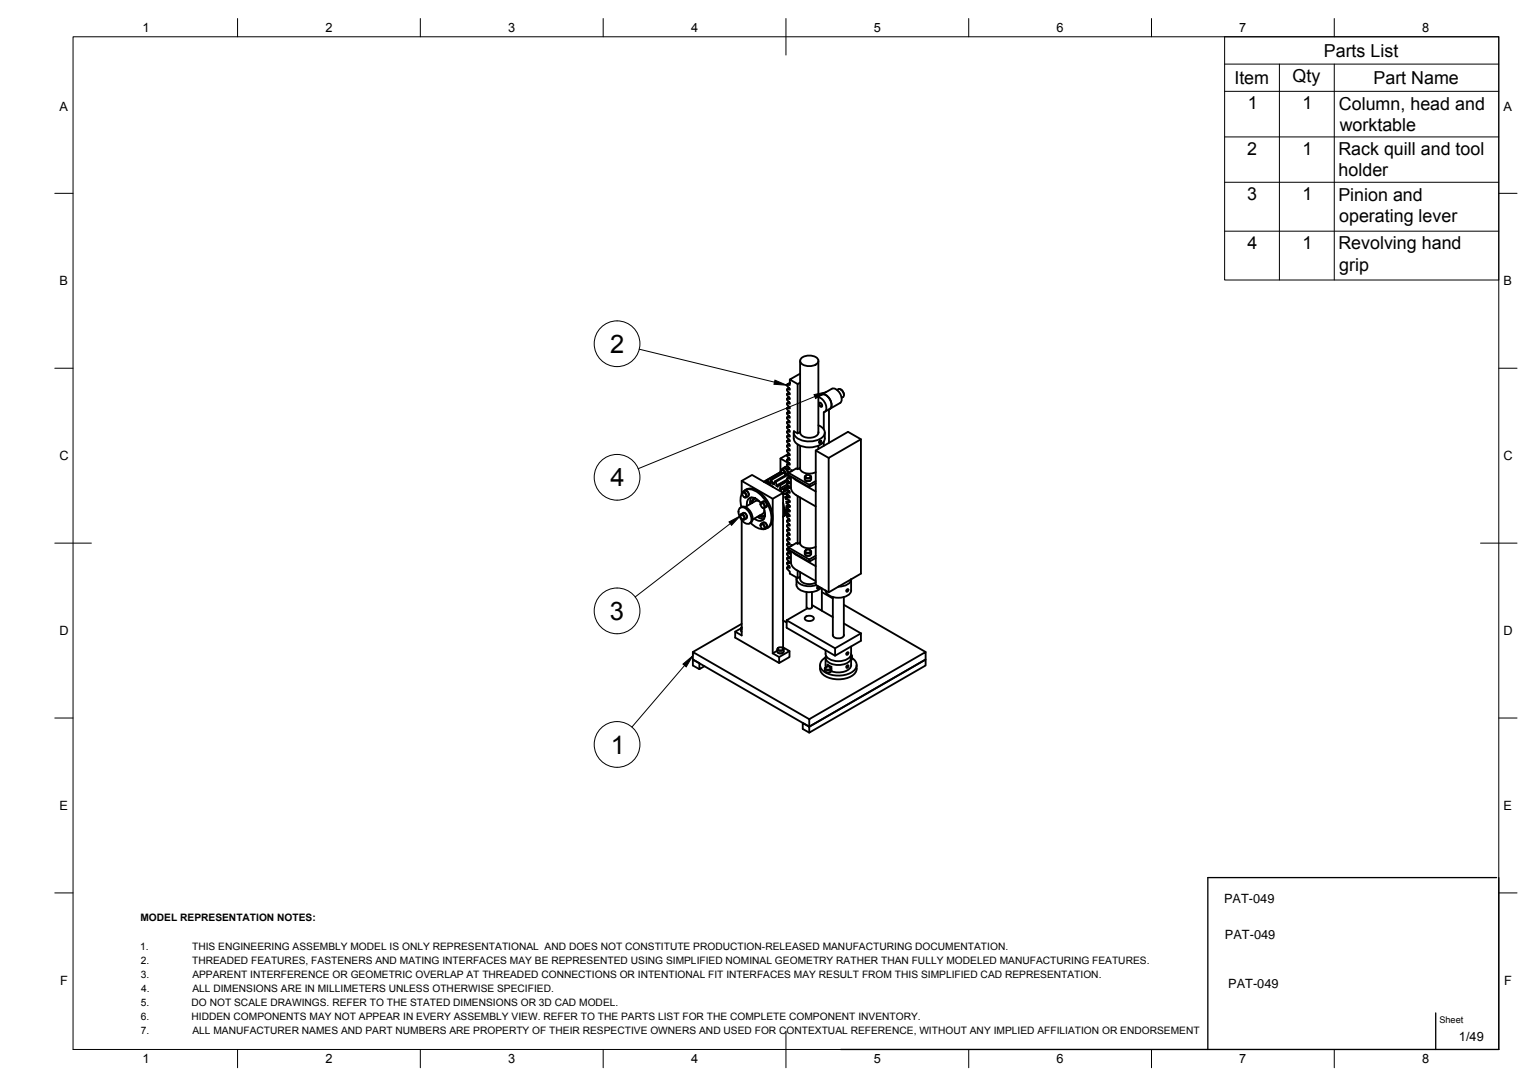
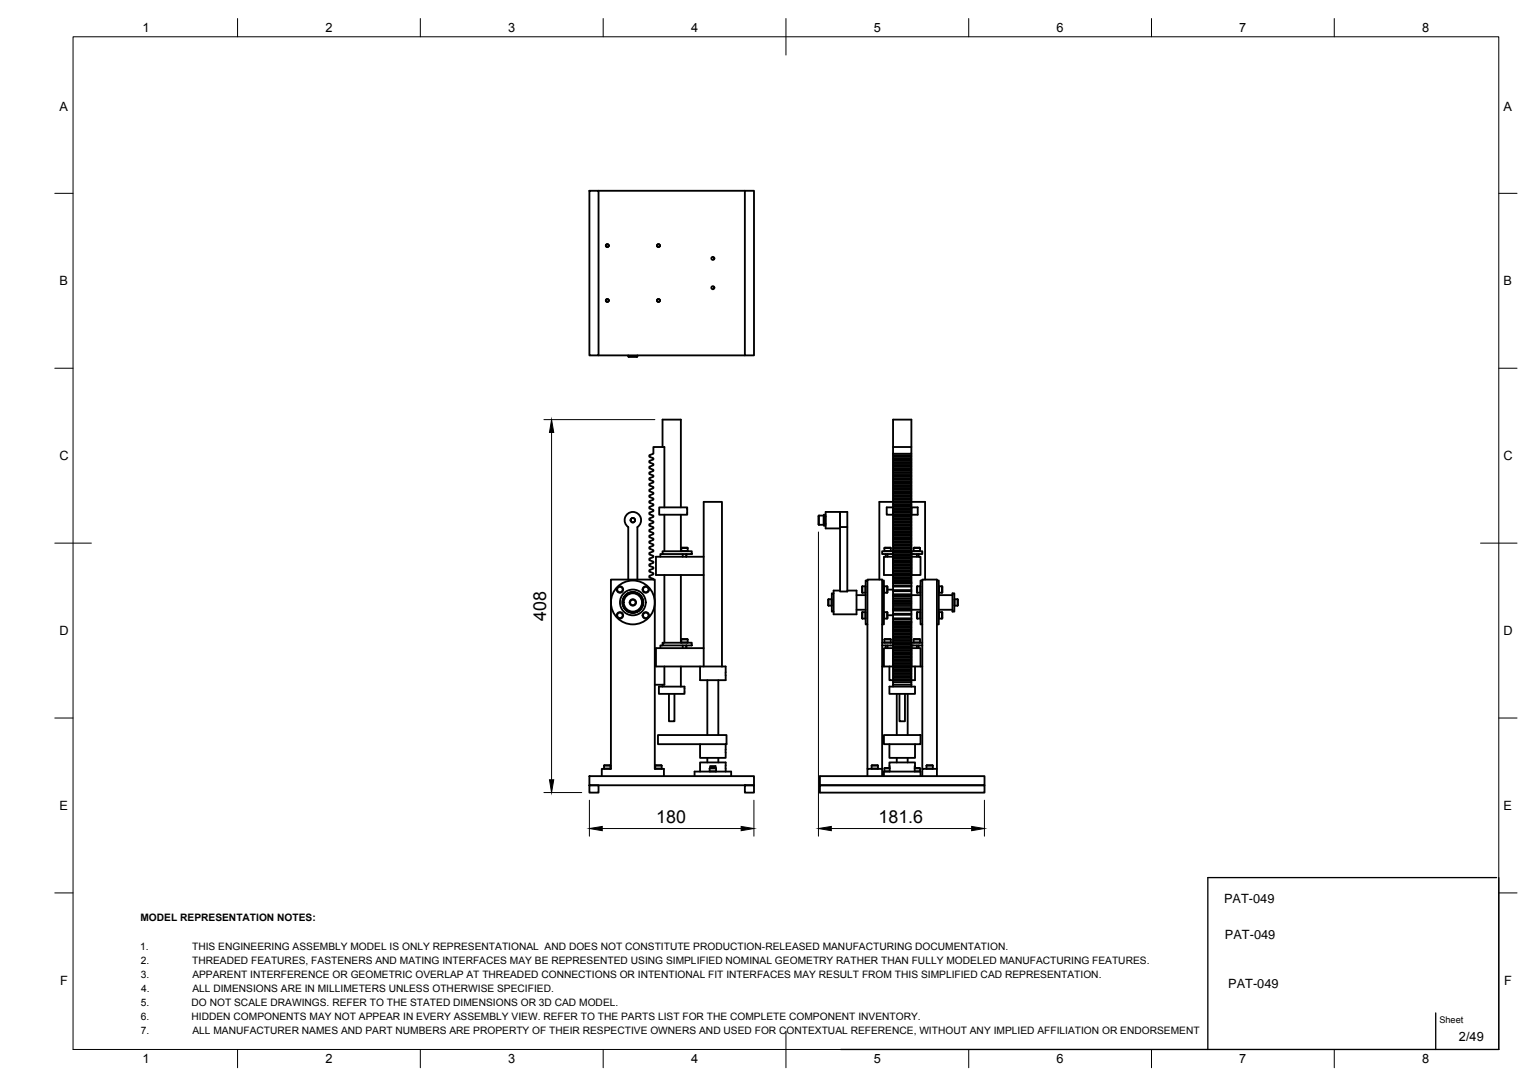
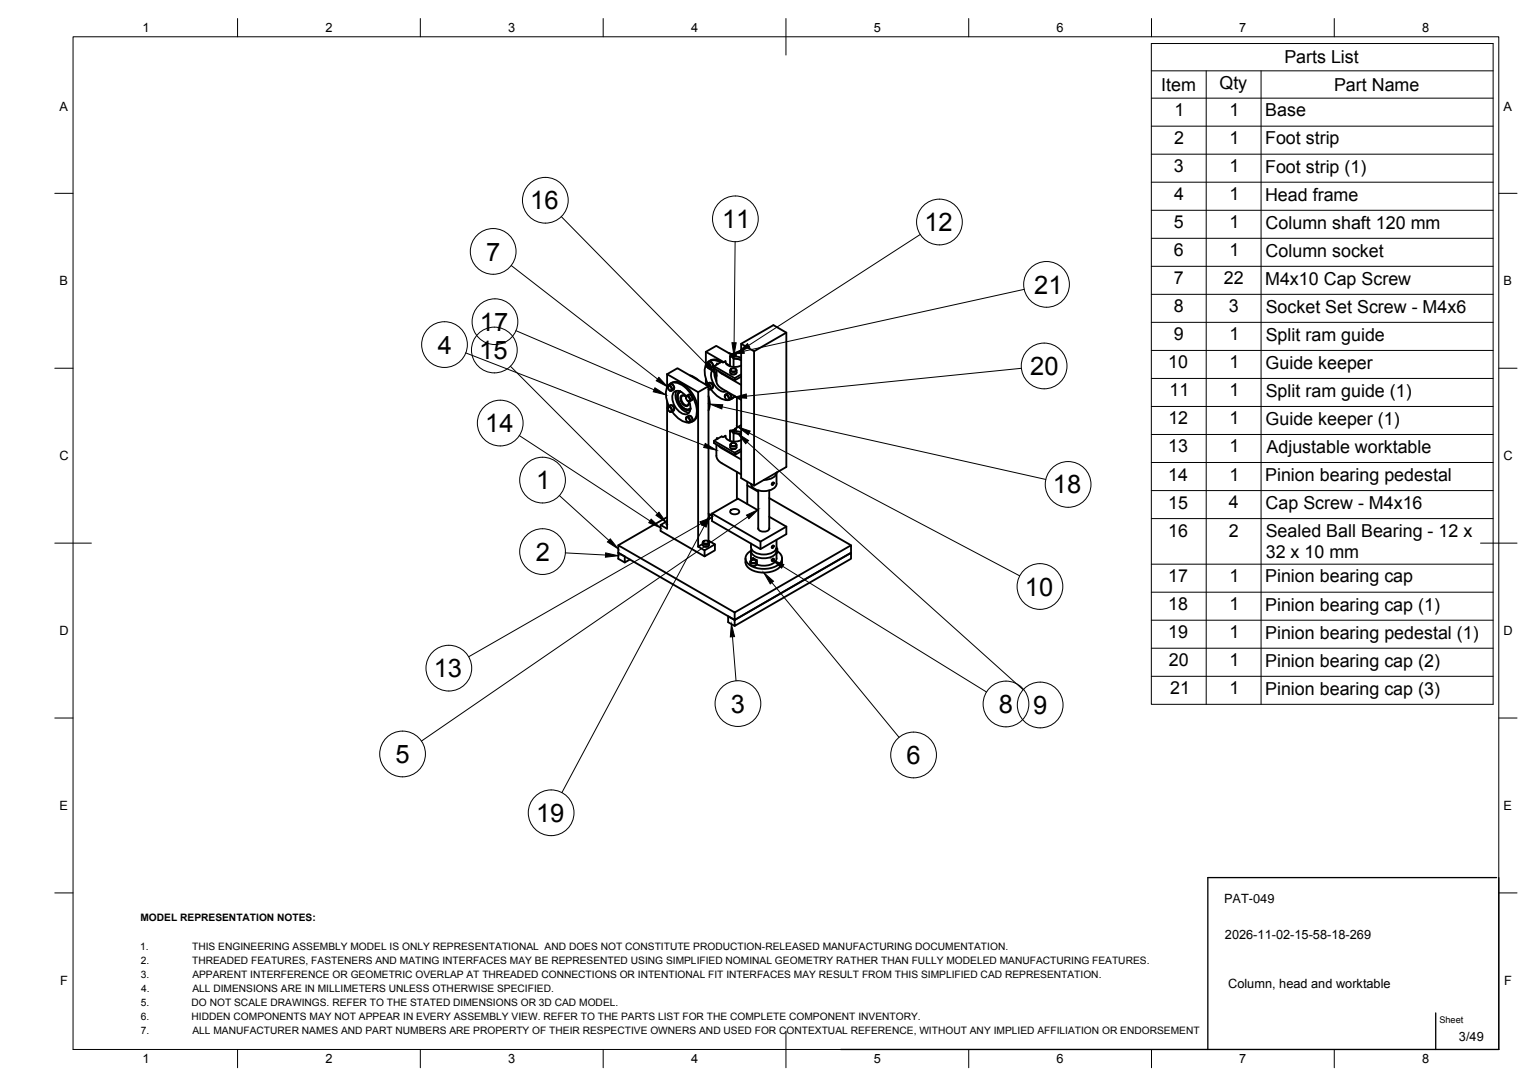
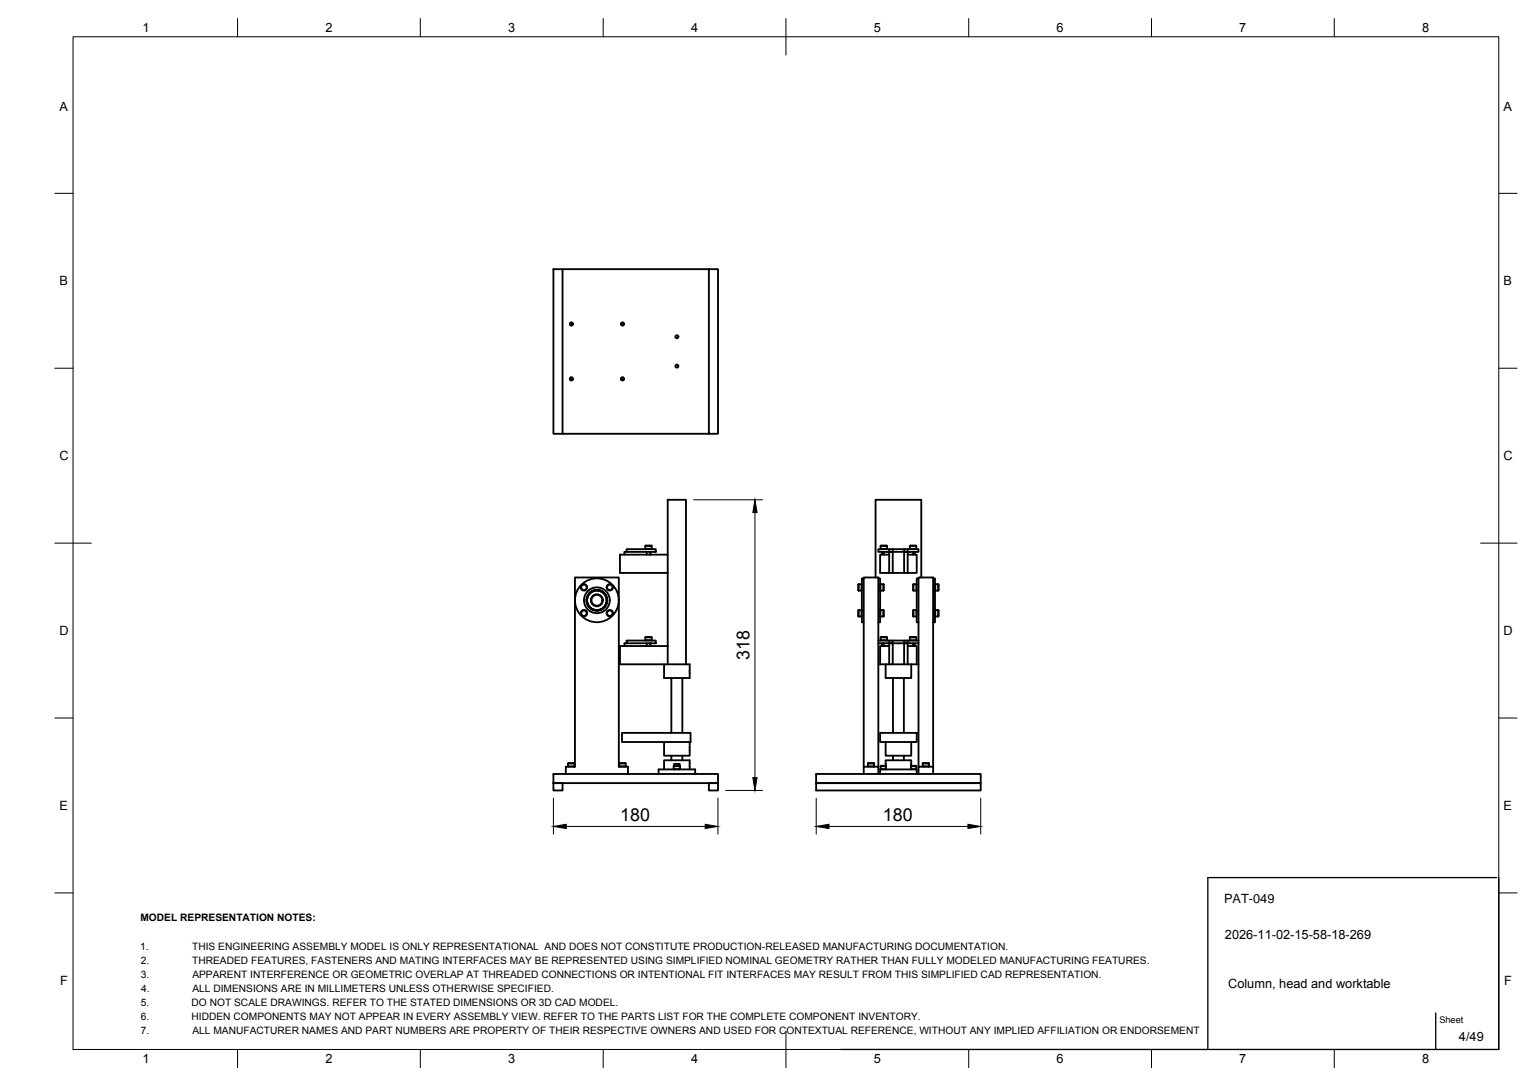
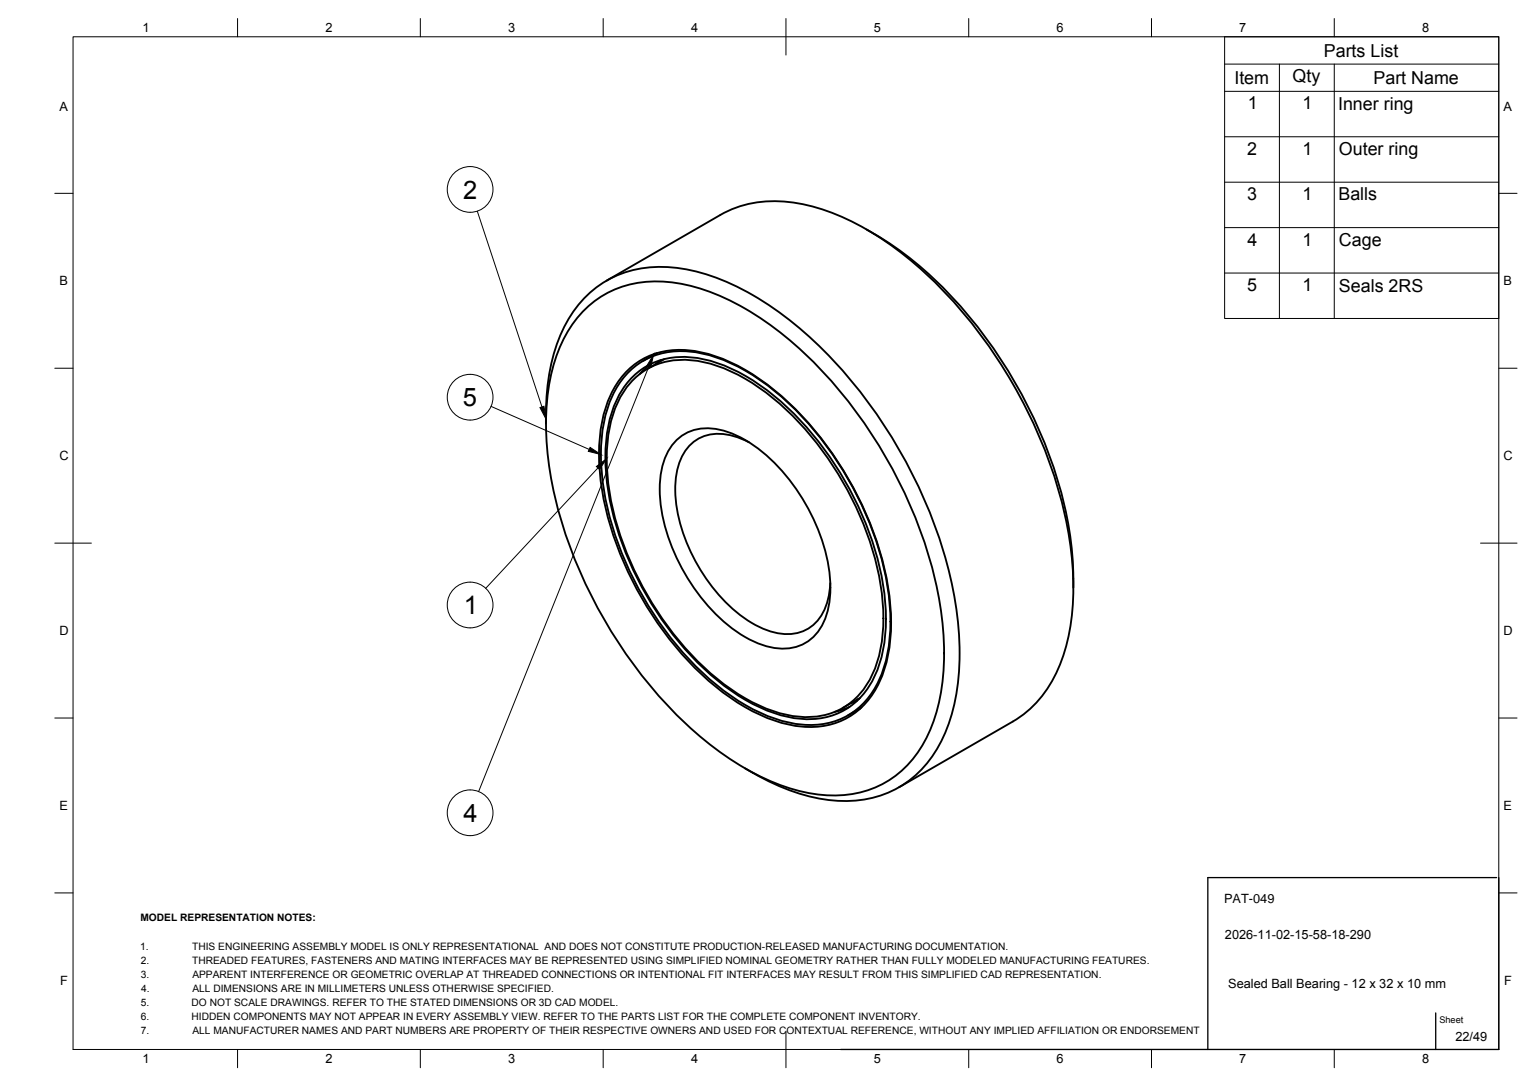
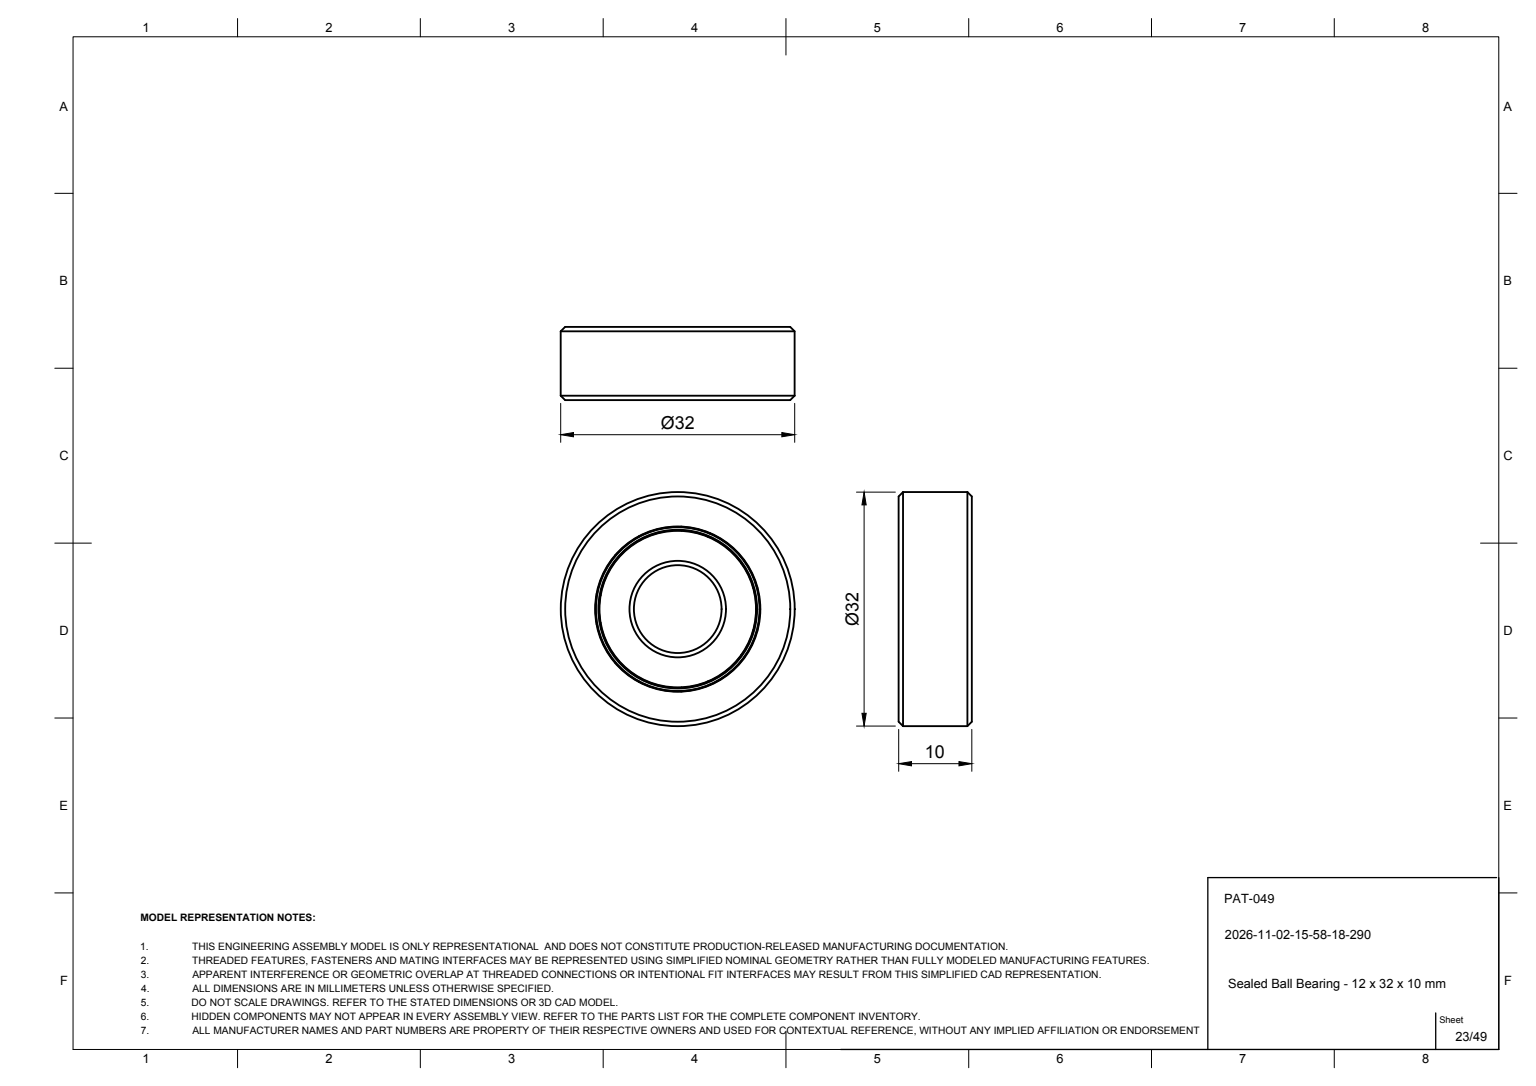
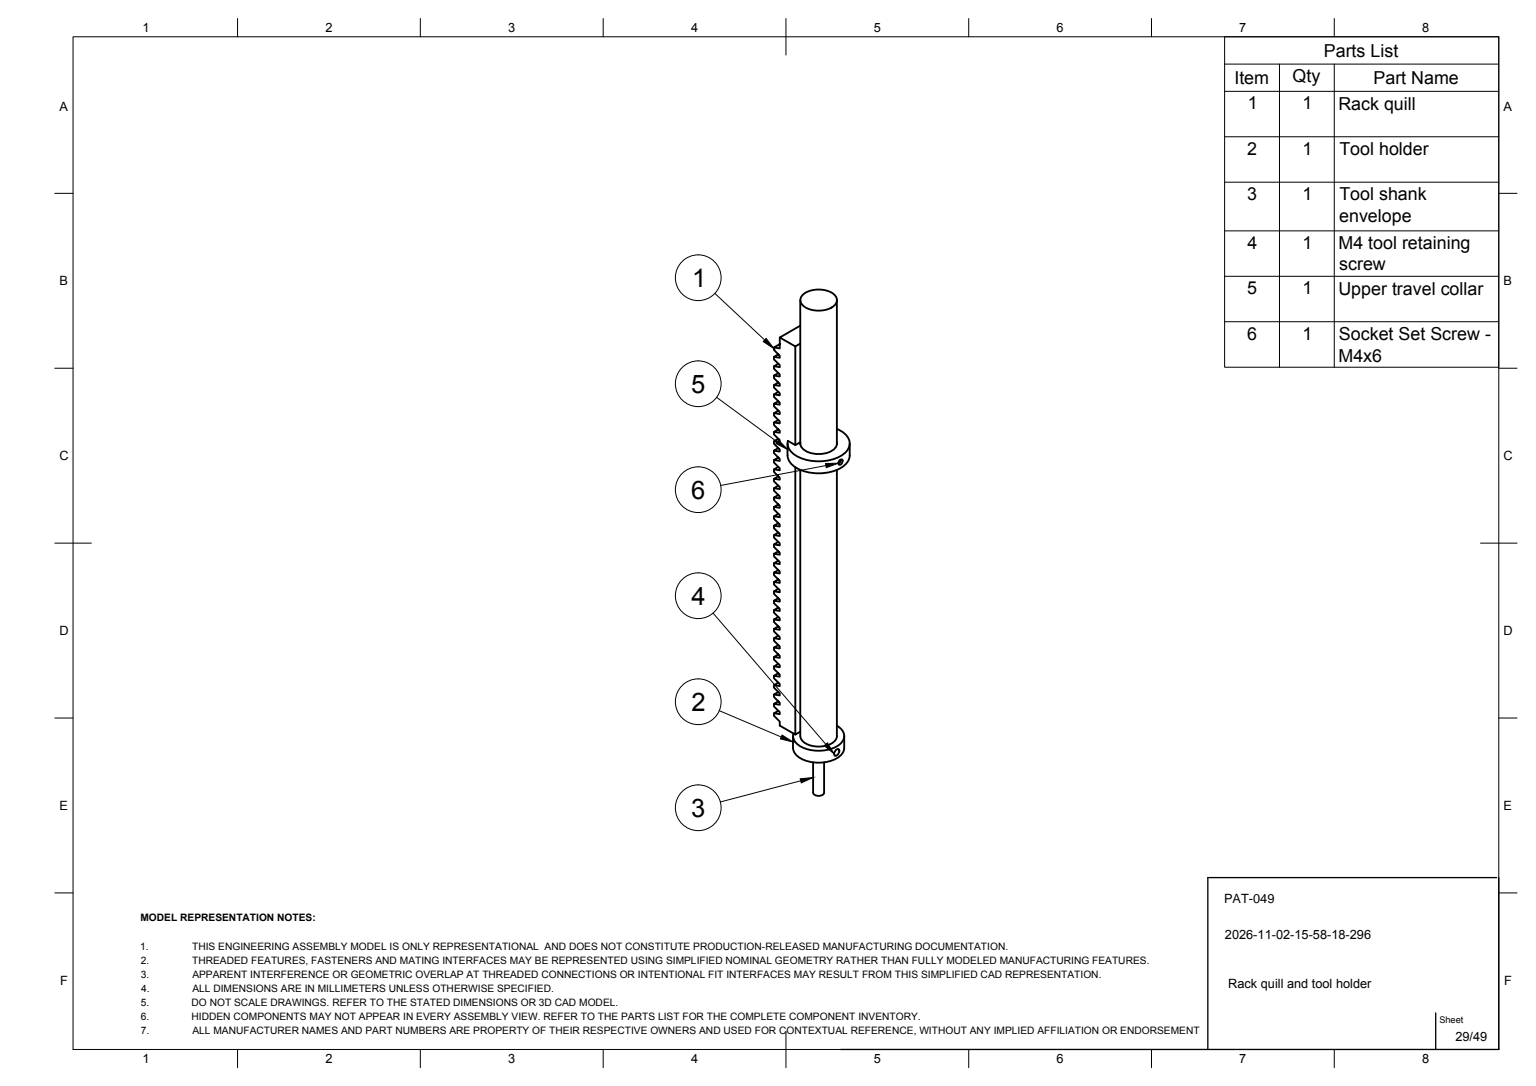
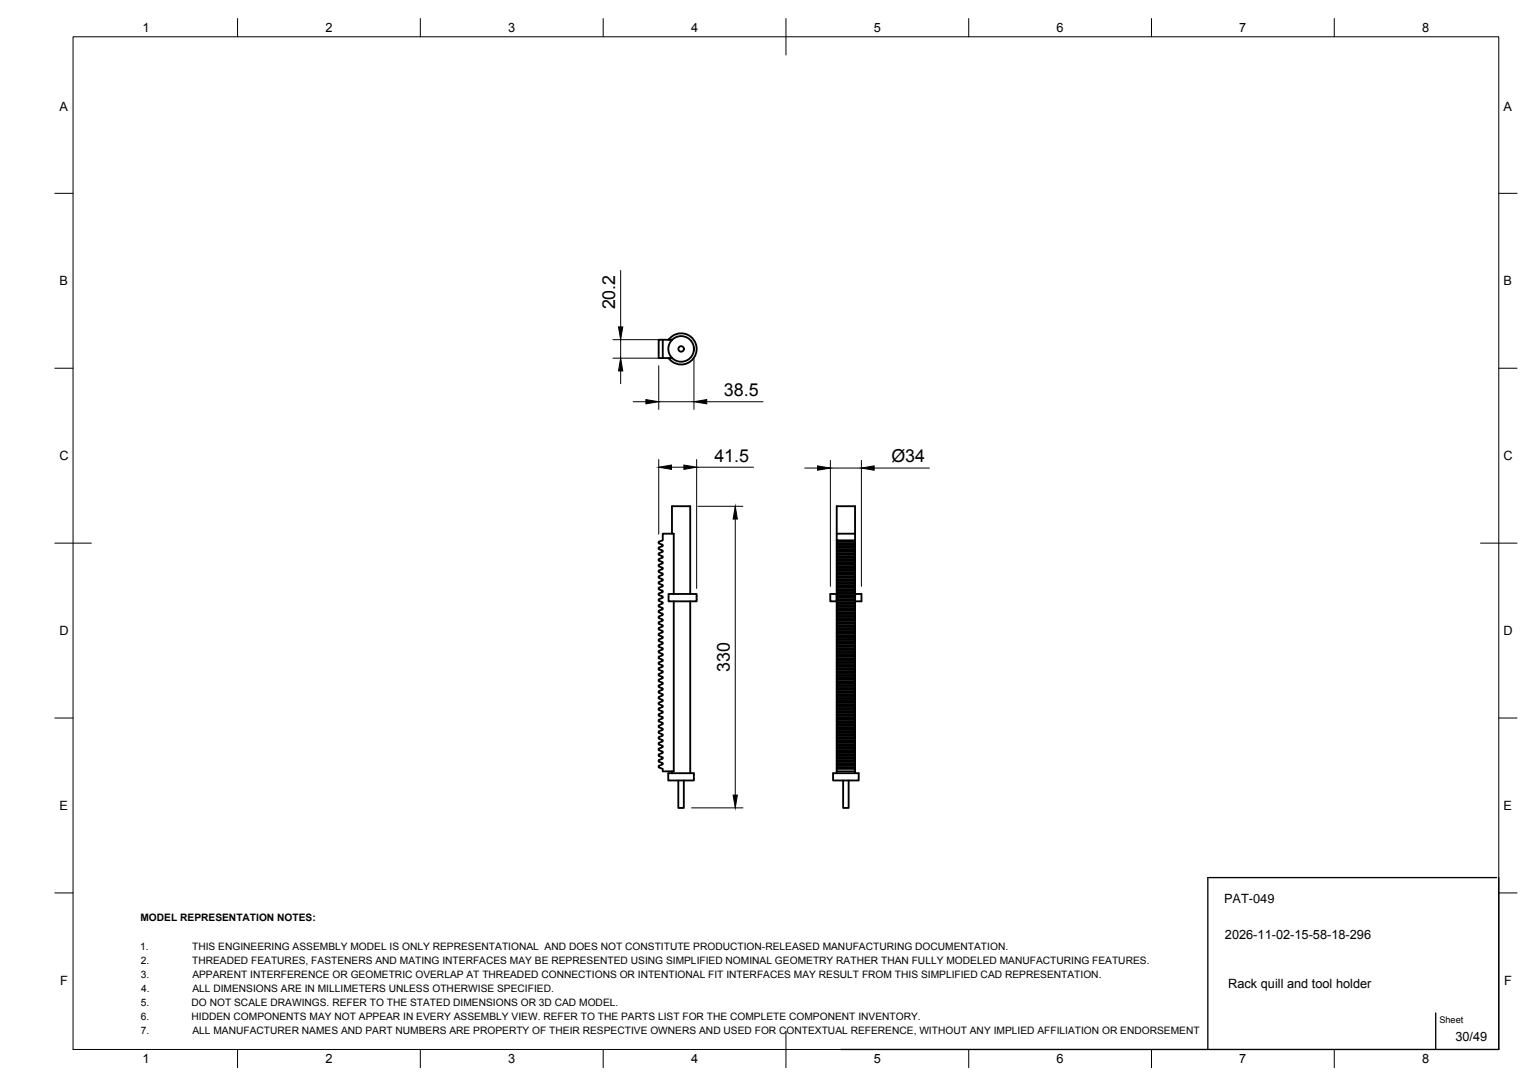
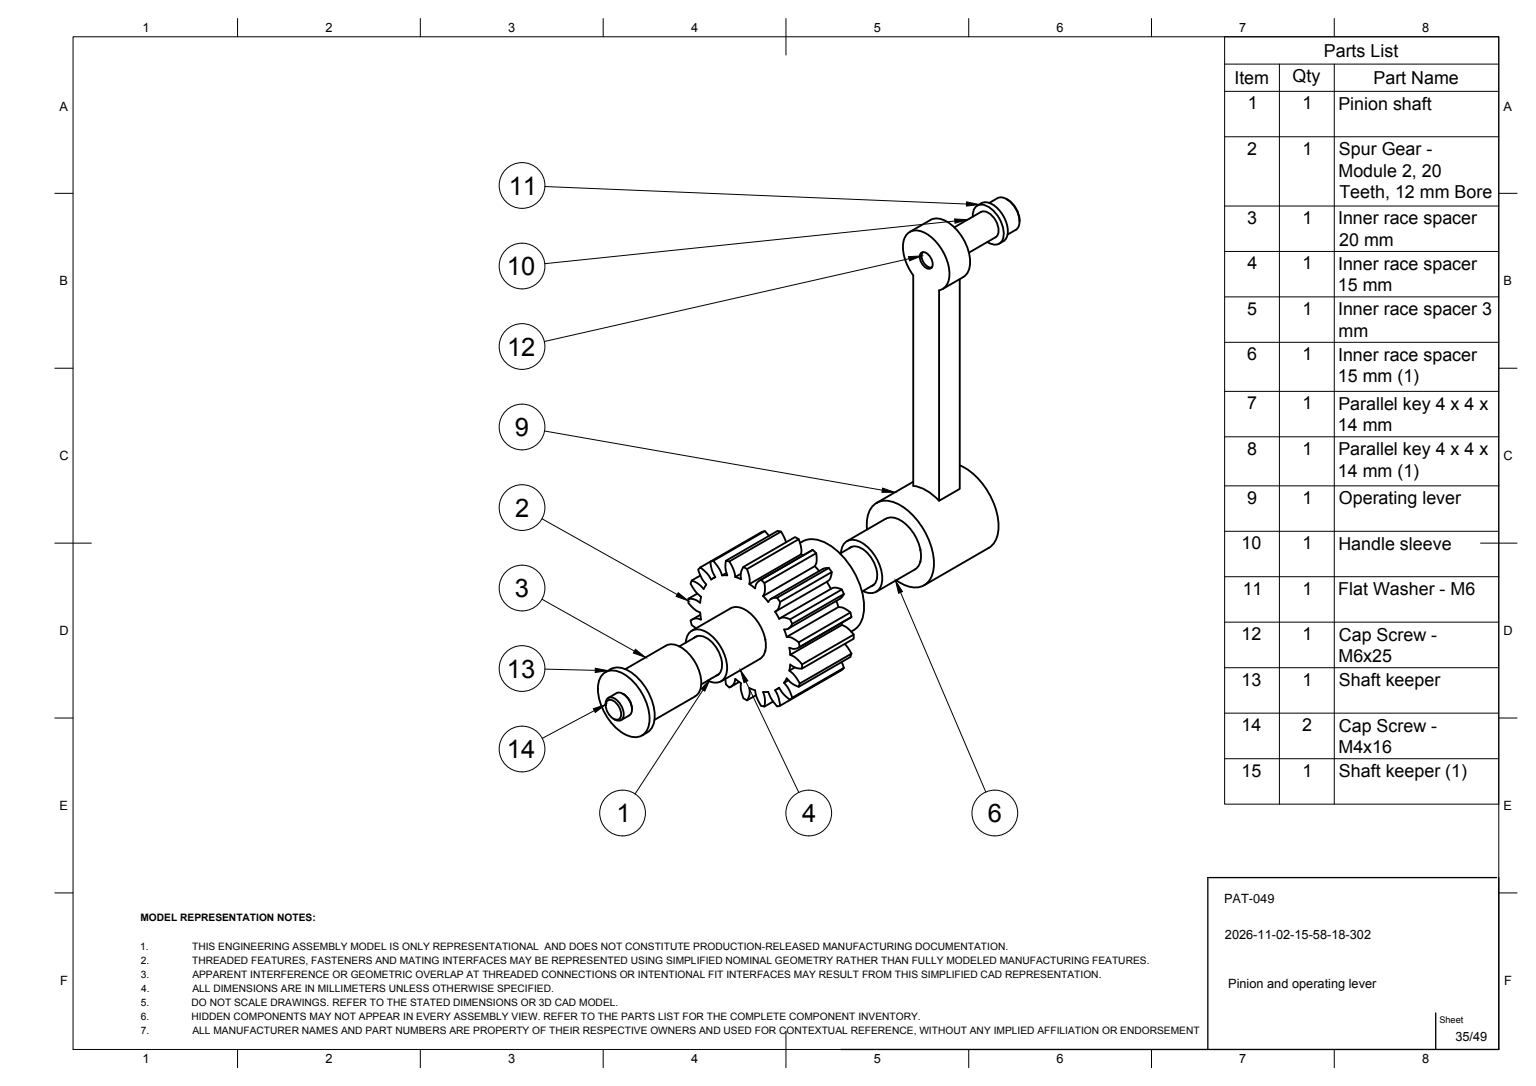
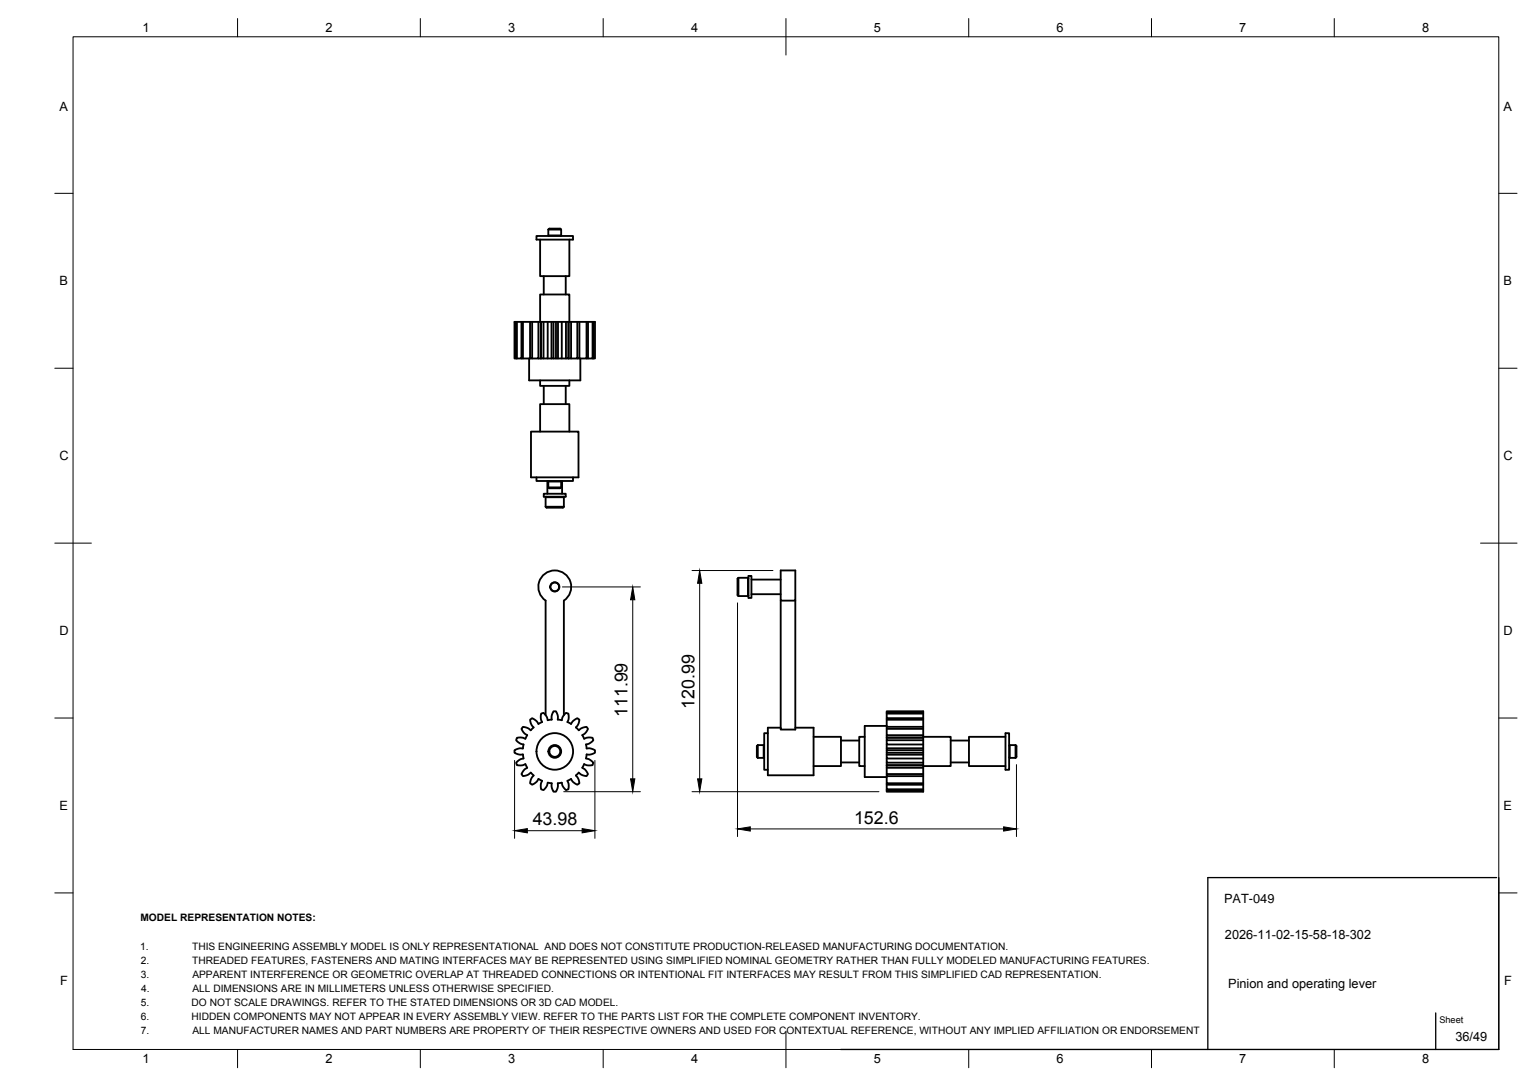
ISO-10303-21;
HEADER;
/* Generated by software containing ST-Developer
 * from STEP Tools, Inc. (www.steptools.com) 
 */

FILE_DESCRIPTION(
/* description */ ('Hand drill press frame (manual)'),
/* implementation_level */ '2;1');

FILE_NAME(
/* name */ 'PAT-049',
/* time_stamp */ '2026-10-28T03:25:28-07:00',
/* author */ (''),
/* organization */ (''),
/* preprocessor_version */ 'ST-DEVELOPER v20.2',
/* originating_system */ 'Autodesk Translation Framework v15.17.0.0',
/* authorisation */ '');

FILE_SCHEMA (('AUTOMOTIVE_DESIGN { 1 0 10303 214 3 1 1 }'));
ENDSEC;

DATA;
#10=MECHANICAL_DESIGN_GEOMETRIC_PRESENTATION_REPRESENTATION('',(#619,#620,
#621,#622,#623,#624,#625,#626,#627,#628,#629,#630,#631,#632,#633,#634,#635,
#636,#637,#638,#639,#640,#641,#642,#643,#644,#645,#646,#647,#648,#649,#650,
#651,#652,#653,#654,#655,#656,#657,#658,#659,#660,#661,#662,#663,#664,#665,
#666,#667,#668,#669,#670),#33299);
#11=(
BOUNDED_SURFACE()
B_SPLINE_SURFACE(5,1,((#24315,#24316),(#24317,#24318),(#24319,#24320),(#24321,
#24322),(#24323,#24324),(#24325,#24326),(#24327,#24328),(#24329,#24330),
(#24331,#24332),(#24333,#24334),(#24335,#24336),(#24337,#24338),(#24339,
#24340),(#24341,#24342),(#24343,#24344),(#24345,#24346),(#24347,#24348),
(#24349,#24350),(#24351,#24352),(#24353,#24354),(#24355,#24356),(#24357,
#24358),(#24359,#24360),(#24361,#24362),(#24363,#24364),(#24365,#24366),
(#24367,#24368),(#24369,#24370),(#24371,#24372),(#24373,#24374),(#24375,
#24376),(#24377,#24378),(#24379,#24380),(#24381,#24382),(#24383,#24384),
(#24385,#24386),(#24387,#24388),(#24389,#24390),(#24391,#24392),(#24393,
#24394),(#24395,#24396),(#24397,#24398),(#24399,#24400),(#24401,#24402),
(#24403,#24404),(#24405,#24406),(#24407,#24408),(#24409,#24410),(#24411,
#24412),(#24413,#24414),(#24415,#24416),(#24417,#24418),(#24419,#24420),
(#24421,#24422),(#24423,#24424),(#24425,#24426),(#24427,#24428),(#24429,
#24430),(#24431,#24432),(#24433,#24434),(#24435,#24436),(#24437,#24438),
(#24439,#24440),(#24441,#24442),(#24443,#24444),(#24445,#24446),(#24447,
#24448),(#24449,#24450),(#24451,#24452),(#24453,#24454)),.UNSPECIFIED.,
 .F.,.F.,.F.)
B_SPLINE_SURFACE_WITH_KNOTS((6,1,1,1,1,1,1,1,1,1,1,1,1,1,1,1,1,1,1,1,1,
1,1,1,1,1,1,1,1,1,1,1,1,1,1,1,1,1,1,1,1,1,1,1,1,1,1,1,1,1,1,1,1,1,1,1,1,
1,1,1,1,1,1,1,1,6),(2,2),(-1.,-0.984615384615383,-0.969230769230768,-0.953846153846152,
-0.938461538461537,-0.923076923076922,-0.907692307692306,-0.892307692307691,
-0.876923076923076,-0.86153846153846,-0.846153846153845,-0.83076923076923,
-0.815384615384614,-0.799999999999999,-0.784615384615384,-0.769230769230768,
-0.753846153846153,-0.738461538461538,-0.723076923076922,-0.707692307692307,
-0.692307692307692,-0.676923076923076,-0.661538461538461,-0.646153846153846,
-0.63076923076923,-0.615384615384615,-0.6,-0.584615384615384,-0.569230769230769,
-0.553846153846154,-0.538461538461538,-0.523076923076923,-0.507692307692308,
-0.492307692307692,-0.476923076923077,-0.461538461538462,-0.446153846153846,
-0.430769230769231,-0.415384615384615,-0.4,-0.384615384615385,-0.369230769230769,
-0.353846153846154,-0.338461538461538,-0.323076923076923,-0.307692307692308,
-0.292307692307692,-0.276923076923077,-0.261538461538462,-0.246153846153846,
-0.230769230769231,-0.215384615384615,-0.2,-0.184615384615385,-0.169230769230769,
-0.153846153846154,-0.138461538461538,-0.123076923076923,-0.107692307692308,
-0.0923076923076923,-0.0769230769230769,-0.0615384615384615,-0.0461538461538462,
-0.0307692307692308,-0.0153846153846154,0.),(-1.,1.),.UNSPECIFIED.)
GEOMETRIC_REPRESENTATION_ITEM()
RATIONAL_B_SPLINE_SURFACE(((1.,1.),(1.,1.),(1.,1.),(1.,1.),(1.,1.),(1.,
1.),(1.,1.),(1.,1.),(1.,1.),(1.,1.),(1.,1.),(1.,1.),(1.,1.),(1.,1.),(1.,
1.),(1.,1.),(1.,1.),(1.,1.),(1.,1.),(1.,1.),(1.,1.),(1.,1.),(1.,1.),(1.,
1.),(1.,1.),(1.,1.),(1.,1.),(1.,1.),(1.,1.),(1.,1.),(1.,1.),(1.,1.),(1.,
1.),(1.,1.),(1.,1.),(1.,1.),(1.,1.),(1.,1.),(1.,1.),(1.,1.),(1.,1.),(1.,
1.),(1.,1.),(1.,1.),(1.,1.),(1.,1.),(1.,1.),(1.,1.),(1.,1.),(1.,1.),(1.,
1.),(1.,1.),(1.,1.),(1.,1.),(1.,1.),(1.,1.),(1.,1.),(1.,1.),(1.,1.),(1.,
1.),(1.,1.),(1.,1.),(1.,1.),(1.,1.),(1.,1.),(1.,1.),(1.,1.),(1.,1.),(1.,
1.),(1.,1.)))
REPRESENTATION_ITEM('')
SURFACE()
);
#12=(
BOUNDED_SURFACE()
B_SPLINE_SURFACE(5,1,((#24533,#24534),(#24535,#24536),(#24537,#24538),(#24539,
#24540),(#24541,#24542),(#24543,#24544),(#24545,#24546),(#24547,#24548),
(#24549,#24550),(#24551,#24552),(#24553,#24554),(#24555,#24556),(#24557,
#24558),(#24559,#24560),(#24561,#24562),(#24563,#24564),(#24565,#24566),
(#24567,#24568),(#24569,#24570),(#24571,#24572),(#24573,#24574),(#24575,
#24576),(#24577,#24578),(#24579,#24580),(#24581,#24582),(#24583,#24584),
(#24585,#24586),(#24587,#24588),(#24589,#24590),(#24591,#24592),(#24593,
#24594),(#24595,#24596),(#24597,#24598),(#24599,#24600),(#24601,#24602),
(#24603,#24604),(#24605,#24606),(#24607,#24608),(#24609,#24610),(#24611,
#24612),(#24613,#24614),(#24615,#24616),(#24617,#24618),(#24619,#24620),
(#24621,#24622),(#24623,#24624),(#24625,#24626),(#24627,#24628),(#24629,
#24630),(#24631,#24632),(#24633,#24634),(#24635,#24636),(#24637,#24638),
(#24639,#24640),(#24641,#24642),(#24643,#24644),(#24645,#24646),(#24647,
#24648),(#24649,#24650),(#24651,#24652),(#24653,#24654),(#24655,#24656),
(#24657,#24658),(#24659,#24660),(#24661,#24662),(#24663,#24664),(#24665,
#24666),(#24667,#24668),(#24669,#24670),(#24671,#24672)),.UNSPECIFIED.,
 .F.,.F.,.F.)
B_SPLINE_SURFACE_WITH_KNOTS((6,1,1,1,1,1,1,1,1,1,1,1,1,1,1,1,1,1,1,1,1,
1,1,1,1,1,1,1,1,1,1,1,1,1,1,1,1,1,1,1,1,1,1,1,1,1,1,1,1,1,1,1,1,1,1,1,1,
1,1,1,1,1,1,1,1,6),(2,2),(-1.,-0.984615384615383,-0.969230769230768,-0.953846153846152,
-0.938461538461537,-0.923076923076922,-0.907692307692306,-0.892307692307691,
-0.876923076923076,-0.86153846153846,-0.846153846153845,-0.83076923076923,
-0.815384615384614,-0.799999999999999,-0.784615384615384,-0.769230769230768,
-0.753846153846153,-0.738461538461538,-0.723076923076922,-0.707692307692307,
-0.692307692307692,-0.676923076923076,-0.661538461538461,-0.646153846153846,
-0.63076923076923,-0.615384615384615,-0.6,-0.584615384615384,-0.569230769230769,
-0.553846153846154,-0.538461538461538,-0.523076923076923,-0.507692307692308,
-0.492307692307692,-0.476923076923077,-0.461538461538462,-0.446153846153846,
-0.430769230769231,-0.415384615384615,-0.4,-0.384615384615385,-0.369230769230769,
-0.353846153846154,-0.338461538461538,-0.323076923076923,-0.307692307692308,
-0.292307692307692,-0.276923076923077,-0.261538461538462,-0.246153846153846,
-0.230769230769231,-0.215384615384615,-0.2,-0.184615384615385,-0.169230769230769,
-0.153846153846154,-0.138461538461538,-0.123076923076923,-0.107692307692308,
-0.0923076923076923,-0.0769230769230769,-0.0615384615384615,-0.0461538461538462,
-0.0307692307692308,-0.0153846153846154,0.),(-1.,1.),.UNSPECIFIED.)
GEOMETRIC_REPRESENTATION_ITEM()
RATIONAL_B_SPLINE_SURFACE(((1.,1.),(1.,1.),(1.,1.),(1.,1.),(1.,1.),(1.,
1.),(1.,1.),(1.,1.),(1.,1.),(1.,1.),(1.,1.),(1.,1.),(1.,1.),(1.,1.),(1.,
1.),(1.,1.),(1.,1.),(1.,1.),(1.,1.),(1.,1.),(1.,1.),(1.,1.),(1.,1.),(1.,
1.),(1.,1.),(1.,1.),(1.,1.),(1.,1.),(1.,1.),(1.,1.),(1.,1.),(1.,1.),(1.,
1.),(1.,1.),(1.,1.),(1.,1.),(1.,1.),(1.,1.),(1.,1.),(1.,1.),(1.,1.),(1.,
1.),(1.,1.),(1.,1.),(1.,1.),(1.,1.),(1.,1.),(1.,1.),(1.,1.),(1.,1.),(1.,
1.),(1.,1.),(1.,1.),(1.,1.),(1.,1.),(1.,1.),(1.,1.),(1.,1.),(1.,1.),(1.,
1.),(1.,1.),(1.,1.),(1.,1.),(1.,1.),(1.,1.),(1.,1.),(1.,1.),(1.,1.),(1.,
1.),(1.,1.)))
REPRESENTATION_ITEM('')
SURFACE()
);
#13=(
BOUNDED_SURFACE()
B_SPLINE_SURFACE(5,1,((#24749,#24750),(#24751,#24752),(#24753,#24754),(#24755,
#24756),(#24757,#24758),(#24759,#24760),(#24761,#24762),(#24763,#24764),
(#24765,#24766),(#24767,#24768),(#24769,#24770),(#24771,#24772),(#24773,
#24774),(#24775,#24776),(#24777,#24778),(#24779,#24780),(#24781,#24782),
(#24783,#24784),(#24785,#24786),(#24787,#24788),(#24789,#24790),(#24791,
#24792),(#24793,#24794),(#24795,#24796),(#24797,#24798),(#24799,#24800),
(#24801,#24802),(#24803,#24804),(#24805,#24806),(#24807,#24808),(#24809,
#24810),(#24811,#24812),(#24813,#24814),(#24815,#24816),(#24817,#24818),
(#24819,#24820),(#24821,#24822),(#24823,#24824),(#24825,#24826),(#24827,
#24828),(#24829,#24830),(#24831,#24832),(#24833,#24834),(#24835,#24836),
(#24837,#24838),(#24839,#24840),(#24841,#24842),(#24843,#24844),(#24845,
#24846),(#24847,#24848),(#24849,#24850),(#24851,#24852),(#24853,#24854),
(#24855,#24856),(#24857,#24858),(#24859,#24860),(#24861,#24862),(#24863,
#24864),(#24865,#24866),(#24867,#24868),(#24869,#24870),(#24871,#24872),
(#24873,#24874),(#24875,#24876),(#24877,#24878),(#24879,#24880),(#24881,
#24882),(#24883,#24884),(#24885,#24886),(#24887,#24888)),.UNSPECIFIED.,
 .F.,.F.,.F.)
B_SPLINE_SURFACE_WITH_KNOTS((6,1,1,1,1,1,1,1,1,1,1,1,1,1,1,1,1,1,1,1,1,
1,1,1,1,1,1,1,1,1,1,1,1,1,1,1,1,1,1,1,1,1,1,1,1,1,1,1,1,1,1,1,1,1,1,1,1,
1,1,1,1,1,1,1,1,6),(2,2),(-1.,-0.984615384615383,-0.969230769230768,-0.953846153846152,
-0.938461538461537,-0.923076923076922,-0.907692307692306,-0.892307692307691,
-0.876923076923076,-0.86153846153846,-0.846153846153845,-0.83076923076923,
-0.815384615384614,-0.799999999999999,-0.784615384615384,-0.769230769230768,
-0.753846153846153,-0.738461538461538,-0.723076923076922,-0.707692307692307,
-0.692307692307692,-0.676923076923076,-0.661538461538461,-0.646153846153846,
-0.63076923076923,-0.615384615384615,-0.6,-0.584615384615384,-0.569230769230769,
-0.553846153846154,-0.538461538461538,-0.523076923076923,-0.507692307692308,
-0.492307692307692,-0.476923076923077,-0.461538461538462,-0.446153846153846,
-0.430769230769231,-0.415384615384615,-0.4,-0.384615384615385,-0.369230769230769,
-0.353846153846154,-0.338461538461538,-0.323076923076923,-0.307692307692308,
-0.292307692307692,-0.276923076923077,-0.261538461538462,-0.246153846153846,
-0.230769230769231,-0.215384615384615,-0.2,-0.184615384615385,-0.169230769230769,
-0.153846153846154,-0.138461538461538,-0.123076923076923,-0.107692307692308,
-0.0923076923076923,-0.0769230769230769,-0.0615384615384615,-0.0461538461538462,
-0.0307692307692308,-0.0153846153846154,0.),(-1.,1.),.UNSPECIFIED.)
GEOMETRIC_REPRESENTATION_ITEM()
RATIONAL_B_SPLINE_SURFACE(((1.,1.),(1.,1.),(1.,1.),(1.,1.),(1.,1.),(1.,
1.),(1.,1.),(1.,1.),(1.,1.),(1.,1.),(1.,1.),(1.,1.),(1.,1.),(1.,1.),(1.,
1.),(1.,1.),(1.,1.),(1.,1.),(1.,1.),(1.,1.),(1.,1.),(1.,1.),(1.,1.),(1.,
1.),(1.,1.),(1.,1.),(1.,1.),(1.,1.),(1.,1.),(1.,1.),(1.,1.),(1.,1.),(1.,
1.),(1.,1.),(1.,1.),(1.,1.),(1.,1.),(1.,1.),(1.,1.),(1.,1.),(1.,1.),(1.,
1.),(1.,1.),(1.,1.),(1.,1.),(1.,1.),(1.,1.),(1.,1.),(1.,1.),(1.,1.),(1.,
1.),(1.,1.),(1.,1.),(1.,1.),(1.,1.),(1.,1.),(1.,1.),(1.,1.),(1.,1.),(1.,
1.),(1.,1.),(1.,1.),(1.,1.),(1.,1.),(1.,1.),(1.,1.),(1.,1.),(1.,1.),(1.,
1.),(1.,1.)))
REPRESENTATION_ITEM('')
SURFACE()
);
#14=(
BOUNDED_SURFACE()
B_SPLINE_SURFACE(5,1,((#24965,#24966),(#24967,#24968),(#24969,#24970),(#24971,
#24972),(#24973,#24974),(#24975,#24976),(#24977,#24978),(#24979,#24980),
(#24981,#24982),(#24983,#24984),(#24985,#24986),(#24987,#24988),(#24989,
#24990),(#24991,#24992),(#24993,#24994),(#24995,#24996),(#24997,#24998),
(#24999,#25000),(#25001,#25002),(#25003,#25004),(#25005,#25006),(#25007,
#25008),(#25009,#25010),(#25011,#25012),(#25013,#25014),(#25015,#25016),
(#25017,#25018),(#25019,#25020),(#25021,#25022),(#25023,#25024),(#25025,
#25026),(#25027,#25028),(#25029,#25030),(#25031,#25032),(#25033,#25034),
(#25035,#25036),(#25037,#25038),(#25039,#25040),(#25041,#25042),(#25043,
#25044),(#25045,#25046),(#25047,#25048),(#25049,#25050),(#25051,#25052),
(#25053,#25054),(#25055,#25056),(#25057,#25058),(#25059,#25060),(#25061,
#25062),(#25063,#25064),(#25065,#25066),(#25067,#25068),(#25069,#25070),
(#25071,#25072),(#25073,#25074),(#25075,#25076),(#25077,#25078),(#25079,
#25080),(#25081,#25082),(#25083,#25084),(#25085,#25086),(#25087,#25088),
(#25089,#25090),(#25091,#25092),(#25093,#25094),(#25095,#25096),(#25097,
#25098),(#25099,#25100),(#25101,#25102),(#25103,#25104)),.UNSPECIFIED.,
 .F.,.F.,.F.)
B_SPLINE_SURFACE_WITH_KNOTS((6,1,1,1,1,1,1,1,1,1,1,1,1,1,1,1,1,1,1,1,1,
1,1,1,1,1,1,1,1,1,1,1,1,1,1,1,1,1,1,1,1,1,1,1,1,1,1,1,1,1,1,1,1,1,1,1,1,
1,1,1,1,1,1,1,1,6),(2,2),(-1.,-0.984615384615383,-0.969230769230768,-0.953846153846152,
-0.938461538461537,-0.923076923076922,-0.907692307692306,-0.892307692307691,
-0.876923076923076,-0.86153846153846,-0.846153846153845,-0.83076923076923,
-0.815384615384614,-0.799999999999999,-0.784615384615384,-0.769230769230768,
-0.753846153846153,-0.738461538461538,-0.723076923076922,-0.707692307692307,
-0.692307692307692,-0.676923076923076,-0.661538461538461,-0.646153846153846,
-0.63076923076923,-0.615384615384615,-0.6,-0.584615384615384,-0.569230769230769,
-0.553846153846154,-0.538461538461538,-0.523076923076923,-0.507692307692308,
-0.492307692307692,-0.476923076923077,-0.461538461538462,-0.446153846153846,
-0.430769230769231,-0.415384615384615,-0.4,-0.384615384615385,-0.369230769230769,
-0.353846153846154,-0.338461538461538,-0.323076923076923,-0.307692307692308,
-0.292307692307692,-0.276923076923077,-0.261538461538462,-0.246153846153846,
-0.230769230769231,-0.215384615384615,-0.2,-0.184615384615385,-0.169230769230769,
-0.153846153846154,-0.138461538461538,-0.123076923076923,-0.107692307692308,
-0.0923076923076923,-0.0769230769230769,-0.0615384615384615,-0.0461538461538462,
-0.0307692307692308,-0.0153846153846154,0.),(-1.,1.),.UNSPECIFIED.)
GEOMETRIC_REPRESENTATION_ITEM()
RATIONAL_B_SPLINE_SURFACE(((1.,1.),(1.,1.),(1.,1.),(1.,1.),(1.,1.),(1.,
1.),(1.,1.),(1.,1.),(1.,1.),(1.,1.),(1.,1.),(1.,1.),(1.,1.),(1.,1.),(1.,
1.),(1.,1.),(1.,1.),(1.,1.),(1.,1.),(1.,1.),(1.,1.),(1.,1.),(1.,1.),(1.,
1.),(1.,1.),(1.,1.),(1.,1.),(1.,1.),(1.,1.),(1.,1.),(1.,1.),(1.,1.),(1.,
1.),(1.,1.),(1.,1.),(1.,1.),(1.,1.),(1.,1.),(1.,1.),(1.,1.),(1.,1.),(1.,
1.),(1.,1.),(1.,1.),(1.,1.),(1.,1.),(1.,1.),(1.,1.),(1.,1.),(1.,1.),(1.,
1.),(1.,1.),(1.,1.),(1.,1.),(1.,1.),(1.,1.),(1.,1.),(1.,1.),(1.,1.),(1.,
1.),(1.,1.),(1.,1.),(1.,1.),(1.,1.),(1.,1.),(1.,1.),(1.,1.),(1.,1.),(1.,
1.),(1.,1.)))
REPRESENTATION_ITEM('')
SURFACE()
);
#15=(
BOUNDED_SURFACE()
B_SPLINE_SURFACE(5,1,((#25181,#25182),(#25183,#25184),(#25185,#25186),(#25187,
#25188),(#25189,#25190),(#25191,#25192),(#25193,#25194),(#25195,#25196),
(#25197,#25198),(#25199,#25200),(#25201,#25202),(#25203,#25204),(#25205,
#25206),(#25207,#25208),(#25209,#25210),(#25211,#25212),(#25213,#25214),
(#25215,#25216),(#25217,#25218),(#25219,#25220),(#25221,#25222),(#25223,
#25224),(#25225,#25226),(#25227,#25228),(#25229,#25230),(#25231,#25232),
(#25233,#25234),(#25235,#25236),(#25237,#25238),(#25239,#25240),(#25241,
#25242),(#25243,#25244),(#25245,#25246),(#25247,#25248),(#25249,#25250),
(#25251,#25252),(#25253,#25254),(#25255,#25256),(#25257,#25258),(#25259,
#25260),(#25261,#25262),(#25263,#25264),(#25265,#25266),(#25267,#25268),
(#25269,#25270),(#25271,#25272),(#25273,#25274),(#25275,#25276),(#25277,
#25278),(#25279,#25280),(#25281,#25282),(#25283,#25284),(#25285,#25286),
(#25287,#25288),(#25289,#25290),(#25291,#25292),(#25293,#25294),(#25295,
#25296),(#25297,#25298),(#25299,#25300),(#25301,#25302),(#25303,#25304),
(#25305,#25306),(#25307,#25308),(#25309,#25310),(#25311,#25312),(#25313,
#25314),(#25315,#25316),(#25317,#25318),(#25319,#25320)),.UNSPECIFIED.,
 .F.,.F.,.F.)
B_SPLINE_SURFACE_WITH_KNOTS((6,1,1,1,1,1,1,1,1,1,1,1,1,1,1,1,1,1,1,1,1,
1,1,1,1,1,1,1,1,1,1,1,1,1,1,1,1,1,1,1,1,1,1,1,1,1,1,1,1,1,1,1,1,1,1,1,1,
1,1,1,1,1,1,1,1,6),(2,2),(-1.,-0.984615384615383,-0.969230769230768,-0.953846153846152,
-0.938461538461537,-0.923076923076922,-0.907692307692306,-0.892307692307691,
-0.876923076923076,-0.86153846153846,-0.846153846153845,-0.83076923076923,
-0.815384615384614,-0.799999999999999,-0.784615384615384,-0.769230769230768,
-0.753846153846153,-0.738461538461538,-0.723076923076922,-0.707692307692307,
-0.692307692307692,-0.676923076923076,-0.661538461538461,-0.646153846153846,
-0.63076923076923,-0.615384615384615,-0.6,-0.584615384615384,-0.569230769230769,
-0.553846153846154,-0.538461538461538,-0.523076923076923,-0.507692307692308,
-0.492307692307692,-0.476923076923077,-0.461538461538462,-0.446153846153846,
-0.430769230769231,-0.415384615384615,-0.4,-0.384615384615385,-0.369230769230769,
-0.353846153846154,-0.338461538461538,-0.323076923076923,-0.307692307692308,
-0.292307692307692,-0.276923076923077,-0.261538461538462,-0.246153846153846,
-0.230769230769231,-0.215384615384615,-0.2,-0.184615384615385,-0.169230769230769,
-0.153846153846154,-0.138461538461538,-0.123076923076923,-0.107692307692308,
-0.0923076923076923,-0.0769230769230769,-0.0615384615384615,-0.0461538461538462,
-0.0307692307692308,-0.0153846153846154,0.),(-1.,1.),.UNSPECIFIED.)
GEOMETRIC_REPRESENTATION_ITEM()
RATIONAL_B_SPLINE_SURFACE(((1.,1.),(1.,1.),(1.,1.),(1.,1.),(1.,1.),(1.,
1.),(1.,1.),(1.,1.),(1.,1.),(1.,1.),(1.,1.),(1.,1.),(1.,1.),(1.,1.),(1.,
1.),(1.,1.),(1.,1.),(1.,1.),(1.,1.),(1.,1.),(1.,1.),(1.,1.),(1.,1.),(1.,
1.),(1.,1.),(1.,1.),(1.,1.),(1.,1.),(1.,1.),(1.,1.),(1.,1.),(1.,1.),(1.,
1.),(1.,1.),(1.,1.),(1.,1.),(1.,1.),(1.,1.),(1.,1.),(1.,1.),(1.,1.),(1.,
1.),(1.,1.),(1.,1.),(1.,1.),(1.,1.),(1.,1.),(1.,1.),(1.,1.),(1.,1.),(1.,
1.),(1.,1.),(1.,1.),(1.,1.),(1.,1.),(1.,1.),(1.,1.),(1.,1.),(1.,1.),(1.,
1.),(1.,1.),(1.,1.),(1.,1.),(1.,1.),(1.,1.),(1.,1.),(1.,1.),(1.,1.),(1.,
1.),(1.,1.)))
REPRESENTATION_ITEM('')
SURFACE()
);
#16=(
BOUNDED_SURFACE()
B_SPLINE_SURFACE(5,1,((#25397,#25398),(#25399,#25400),(#25401,#25402),(#25403,
#25404),(#25405,#25406),(#25407,#25408),(#25409,#25410),(#25411,#25412),
(#25413,#25414),(#25415,#25416),(#25417,#25418),(#25419,#25420),(#25421,
#25422),(#25423,#25424),(#25425,#25426),(#25427,#25428),(#25429,#25430),
(#25431,#25432),(#25433,#25434),(#25435,#25436),(#25437,#25438),(#25439,
#25440),(#25441,#25442),(#25443,#25444),(#25445,#25446),(#25447,#25448),
(#25449,#25450),(#25451,#25452),(#25453,#25454),(#25455,#25456),(#25457,
#25458),(#25459,#25460),(#25461,#25462),(#25463,#25464),(#25465,#25466),
(#25467,#25468),(#25469,#25470),(#25471,#25472),(#25473,#25474),(#25475,
#25476),(#25477,#25478),(#25479,#25480),(#25481,#25482),(#25483,#25484),
(#25485,#25486),(#25487,#25488),(#25489,#25490),(#25491,#25492),(#25493,
#25494),(#25495,#25496),(#25497,#25498),(#25499,#25500),(#25501,#25502),
(#25503,#25504),(#25505,#25506),(#25507,#25508),(#25509,#25510),(#25511,
#25512),(#25513,#25514),(#25515,#25516),(#25517,#25518),(#25519,#25520),
(#25521,#25522),(#25523,#25524),(#25525,#25526),(#25527,#25528),(#25529,
#25530),(#25531,#25532),(#25533,#25534),(#25535,#25536)),.UNSPECIFIED.,
 .F.,.F.,.F.)
B_SPLINE_SURFACE_WITH_KNOTS((6,1,1,1,1,1,1,1,1,1,1,1,1,1,1,1,1,1,1,1,1,
1,1,1,1,1,1,1,1,1,1,1,1,1,1,1,1,1,1,1,1,1,1,1,1,1,1,1,1,1,1,1,1,1,1,1,1,
1,1,1,1,1,1,1,1,6),(2,2),(-1.,-0.984615384615383,-0.969230769230768,-0.953846153846152,
-0.938461538461537,-0.923076923076922,-0.907692307692306,-0.892307692307691,
-0.876923076923076,-0.86153846153846,-0.846153846153845,-0.83076923076923,
-0.815384615384614,-0.799999999999999,-0.784615384615384,-0.769230769230768,
-0.753846153846153,-0.738461538461538,-0.723076923076922,-0.707692307692307,
-0.692307692307692,-0.676923076923076,-0.661538461538461,-0.646153846153846,
-0.63076923076923,-0.615384615384615,-0.6,-0.584615384615384,-0.569230769230769,
-0.553846153846154,-0.538461538461538,-0.523076923076923,-0.507692307692308,
-0.492307692307692,-0.476923076923077,-0.461538461538462,-0.446153846153846,
-0.430769230769231,-0.415384615384615,-0.4,-0.384615384615385,-0.369230769230769,
-0.353846153846154,-0.338461538461538,-0.323076923076923,-0.307692307692308,
-0.292307692307692,-0.276923076923077,-0.261538461538462,-0.246153846153846,
-0.230769230769231,-0.215384615384615,-0.2,-0.184615384615385,-0.169230769230769,
-0.153846153846154,-0.138461538461538,-0.123076923076923,-0.107692307692308,
-0.0923076923076923,-0.0769230769230769,-0.0615384615384615,-0.0461538461538462,
-0.0307692307692308,-0.0153846153846154,0.),(-1.,1.),.UNSPECIFIED.)
GEOMETRIC_REPRESENTATION_ITEM()
RATIONAL_B_SPLINE_SURFACE(((1.,1.),(1.,1.),(1.,1.),(1.,1.),(1.,1.),(1.,
1.),(1.,1.),(1.,1.),(1.,1.),(1.,1.),(1.,1.),(1.,1.),(1.,1.),(1.,1.),(1.,
1.),(1.,1.),(1.,1.),(1.,1.),(1.,1.),(1.,1.),(1.,1.),(1.,1.),(1.,1.),(1.,
1.),(1.,1.),(1.,1.),(1.,1.),(1.,1.),(1.,1.),(1.,1.),(1.,1.),(1.,1.),(1.,
1.),(1.,1.),(1.,1.),(1.,1.),(1.,1.),(1.,1.),(1.,1.),(1.,1.),(1.,1.),(1.,
1.),(1.,1.),(1.,1.),(1.,1.),(1.,1.),(1.,1.),(1.,1.),(1.,1.),(1.,1.),(1.,
1.),(1.,1.),(1.,1.),(1.,1.),(1.,1.),(1.,1.),(1.,1.),(1.,1.),(1.,1.),(1.,
1.),(1.,1.),(1.,1.),(1.,1.),(1.,1.),(1.,1.),(1.,1.),(1.,1.),(1.,1.),(1.,
1.),(1.,1.)))
REPRESENTATION_ITEM('')
SURFACE()
);
#17=(
BOUNDED_SURFACE()
B_SPLINE_SURFACE(5,1,((#25613,#25614),(#25615,#25616),(#25617,#25618),(#25619,
#25620),(#25621,#25622),(#25623,#25624),(#25625,#25626),(#25627,#25628),
(#25629,#25630),(#25631,#25632),(#25633,#25634),(#25635,#25636),(#25637,
#25638),(#25639,#25640),(#25641,#25642),(#25643,#25644),(#25645,#25646),
(#25647,#25648),(#25649,#25650),(#25651,#25652),(#25653,#25654),(#25655,
#25656),(#25657,#25658),(#25659,#25660),(#25661,#25662),(#25663,#25664),
(#25665,#25666),(#25667,#25668),(#25669,#25670),(#25671,#25672),(#25673,
#25674),(#25675,#25676),(#25677,#25678),(#25679,#25680),(#25681,#25682),
(#25683,#25684),(#25685,#25686),(#25687,#25688),(#25689,#25690),(#25691,
#25692),(#25693,#25694),(#25695,#25696),(#25697,#25698),(#25699,#25700),
(#25701,#25702),(#25703,#25704),(#25705,#25706),(#25707,#25708),(#25709,
#25710),(#25711,#25712),(#25713,#25714),(#25715,#25716),(#25717,#25718),
(#25719,#25720),(#25721,#25722),(#25723,#25724),(#25725,#25726),(#25727,
#25728),(#25729,#25730),(#25731,#25732),(#25733,#25734),(#25735,#25736),
(#25737,#25738),(#25739,#25740),(#25741,#25742),(#25743,#25744),(#25745,
#25746),(#25747,#25748),(#25749,#25750),(#25751,#25752)),.UNSPECIFIED.,
 .F.,.F.,.F.)
B_SPLINE_SURFACE_WITH_KNOTS((6,1,1,1,1,1,1,1,1,1,1,1,1,1,1,1,1,1,1,1,1,
1,1,1,1,1,1,1,1,1,1,1,1,1,1,1,1,1,1,1,1,1,1,1,1,1,1,1,1,1,1,1,1,1,1,1,1,
1,1,1,1,1,1,1,1,6),(2,2),(-1.,-0.984615384615383,-0.969230769230768,-0.953846153846152,
-0.938461538461537,-0.923076923076922,-0.907692307692306,-0.892307692307691,
-0.876923076923076,-0.86153846153846,-0.846153846153845,-0.83076923076923,
-0.815384615384614,-0.799999999999999,-0.784615384615384,-0.769230769230768,
-0.753846153846153,-0.738461538461538,-0.723076923076922,-0.707692307692307,
-0.692307692307692,-0.676923076923076,-0.661538461538461,-0.646153846153846,
-0.63076923076923,-0.615384615384615,-0.6,-0.584615384615384,-0.569230769230769,
-0.553846153846154,-0.538461538461538,-0.523076923076923,-0.507692307692308,
-0.492307692307692,-0.476923076923077,-0.461538461538462,-0.446153846153846,
-0.430769230769231,-0.415384615384615,-0.4,-0.384615384615385,-0.369230769230769,
-0.353846153846154,-0.338461538461538,-0.323076923076923,-0.307692307692308,
-0.292307692307692,-0.276923076923077,-0.261538461538462,-0.246153846153846,
-0.230769230769231,-0.215384615384615,-0.2,-0.184615384615385,-0.169230769230769,
-0.153846153846154,-0.138461538461538,-0.123076923076923,-0.107692307692308,
-0.0923076923076923,-0.0769230769230769,-0.0615384615384615,-0.0461538461538462,
-0.0307692307692308,-0.0153846153846154,0.),(-1.,1.),.UNSPECIFIED.)
GEOMETRIC_REPRESENTATION_ITEM()
RATIONAL_B_SPLINE_SURFACE(((1.,1.),(1.,1.),(1.,1.),(1.,1.),(1.,1.),(1.,
1.),(1.,1.),(1.,1.),(1.,1.),(1.,1.),(1.,1.),(1.,1.),(1.,1.),(1.,1.),(1.,
1.),(1.,1.),(1.,1.),(1.,1.),(1.,1.),(1.,1.),(1.,1.),(1.,1.),(1.,1.),(1.,
1.),(1.,1.),(1.,1.),(1.,1.),(1.,1.),(1.,1.),(1.,1.),(1.,1.),(1.,1.),(1.,
1.),(1.,1.),(1.,1.),(1.,1.),(1.,1.),(1.,1.),(1.,1.),(1.,1.),(1.,1.),(1.,
1.),(1.,1.),(1.,1.),(1.,1.),(1.,1.),(1.,1.),(1.,1.),(1.,1.),(1.,1.),(1.,
1.),(1.,1.),(1.,1.),(1.,1.),(1.,1.),(1.,1.),(1.,1.),(1.,1.),(1.,1.),(1.,
1.),(1.,1.),(1.,1.),(1.,1.),(1.,1.),(1.,1.),(1.,1.),(1.,1.),(1.,1.),(1.,
1.),(1.,1.)))
REPRESENTATION_ITEM('')
SURFACE()
);
#18=(
BOUNDED_SURFACE()
B_SPLINE_SURFACE(5,1,((#25829,#25830),(#25831,#25832),(#25833,#25834),(#25835,
#25836),(#25837,#25838),(#25839,#25840),(#25841,#25842),(#25843,#25844),
(#25845,#25846),(#25847,#25848),(#25849,#25850),(#25851,#25852),(#25853,
#25854),(#25855,#25856),(#25857,#25858),(#25859,#25860),(#25861,#25862),
(#25863,#25864),(#25865,#25866),(#25867,#25868),(#25869,#25870),(#25871,
#25872),(#25873,#25874),(#25875,#25876),(#25877,#25878),(#25879,#25880),
(#25881,#25882),(#25883,#25884),(#25885,#25886),(#25887,#25888),(#25889,
#25890),(#25891,#25892),(#25893,#25894),(#25895,#25896),(#25897,#25898),
(#25899,#25900),(#25901,#25902),(#25903,#25904),(#25905,#25906),(#25907,
#25908),(#25909,#25910),(#25911,#25912),(#25913,#25914),(#25915,#25916),
(#25917,#25918),(#25919,#25920),(#25921,#25922),(#25923,#25924),(#25925,
#25926),(#25927,#25928),(#25929,#25930),(#25931,#25932),(#25933,#25934),
(#25935,#25936),(#25937,#25938),(#25939,#25940),(#25941,#25942),(#25943,
#25944),(#25945,#25946),(#25947,#25948),(#25949,#25950),(#25951,#25952),
(#25953,#25954),(#25955,#25956),(#25957,#25958),(#25959,#25960),(#25961,
#25962),(#25963,#25964),(#25965,#25966),(#25967,#25968)),.UNSPECIFIED.,
 .F.,.F.,.F.)
B_SPLINE_SURFACE_WITH_KNOTS((6,1,1,1,1,1,1,1,1,1,1,1,1,1,1,1,1,1,1,1,1,
1,1,1,1,1,1,1,1,1,1,1,1,1,1,1,1,1,1,1,1,1,1,1,1,1,1,1,1,1,1,1,1,1,1,1,1,
1,1,1,1,1,1,1,1,6),(2,2),(-1.,-0.984615384615383,-0.969230769230768,-0.953846153846152,
-0.938461538461537,-0.923076923076922,-0.907692307692306,-0.892307692307691,
-0.876923076923076,-0.86153846153846,-0.846153846153845,-0.83076923076923,
-0.815384615384614,-0.799999999999999,-0.784615384615384,-0.769230769230768,
-0.753846153846153,-0.738461538461538,-0.723076923076922,-0.707692307692307,
-0.692307692307692,-0.676923076923076,-0.661538461538461,-0.646153846153846,
-0.63076923076923,-0.615384615384615,-0.6,-0.584615384615384,-0.569230769230769,
-0.553846153846154,-0.538461538461538,-0.523076923076923,-0.507692307692308,
-0.492307692307692,-0.476923076923077,-0.461538461538462,-0.446153846153846,
-0.430769230769231,-0.415384615384615,-0.4,-0.384615384615385,-0.369230769230769,
-0.353846153846154,-0.338461538461538,-0.323076923076923,-0.307692307692308,
-0.292307692307692,-0.276923076923077,-0.261538461538462,-0.246153846153846,
-0.230769230769231,-0.215384615384615,-0.2,-0.184615384615385,-0.169230769230769,
-0.153846153846154,-0.138461538461538,-0.123076923076923,-0.107692307692308,
-0.0923076923076923,-0.0769230769230769,-0.0615384615384615,-0.0461538461538462,
-0.0307692307692308,-0.0153846153846154,0.),(-1.,1.),.UNSPECIFIED.)
GEOMETRIC_REPRESENTATION_ITEM()
RATIONAL_B_SPLINE_SURFACE(((1.,1.),(1.,1.),(1.,1.),(1.,1.),(1.,1.),(1.,
1.),(1.,1.),(1.,1.),(1.,1.),(1.,1.),(1.,1.),(1.,1.),(1.,1.),(1.,1.),(1.,
1.),(1.,1.),(1.,1.),(1.,1.),(1.,1.),(1.,1.),(1.,1.),(1.,1.),(1.,1.),(1.,
1.),(1.,1.),(1.,1.),(1.,1.),(1.,1.),(1.,1.),(1.,1.),(1.,1.),(1.,1.),(1.,
1.),(1.,1.),(1.,1.),(1.,1.),(1.,1.),(1.,1.),(1.,1.),(1.,1.),(1.,1.),(1.,
1.),(1.,1.),(1.,1.),(1.,1.),(1.,1.),(1.,1.),(1.,1.),(1.,1.),(1.,1.),(1.,
1.),(1.,1.),(1.,1.),(1.,1.),(1.,1.),(1.,1.),(1.,1.),(1.,1.),(1.,1.),(1.,
1.),(1.,1.),(1.,1.),(1.,1.),(1.,1.),(1.,1.),(1.,1.),(1.,1.),(1.,1.),(1.,
1.),(1.,1.)))
REPRESENTATION_ITEM('')
SURFACE()
);
#19=(
BOUNDED_SURFACE()
B_SPLINE_SURFACE(5,1,((#26045,#26046),(#26047,#26048),(#26049,#26050),(#26051,
#26052),(#26053,#26054),(#26055,#26056),(#26057,#26058),(#26059,#26060),
(#26061,#26062),(#26063,#26064),(#26065,#26066),(#26067,#26068),(#26069,
#26070),(#26071,#26072),(#26073,#26074),(#26075,#26076),(#26077,#26078),
(#26079,#26080),(#26081,#26082),(#26083,#26084),(#26085,#26086),(#26087,
#26088),(#26089,#26090),(#26091,#26092),(#26093,#26094),(#26095,#26096),
(#26097,#26098),(#26099,#26100),(#26101,#26102),(#26103,#26104),(#26105,
#26106),(#26107,#26108),(#26109,#26110),(#26111,#26112),(#26113,#26114),
(#26115,#26116),(#26117,#26118),(#26119,#26120),(#26121,#26122),(#26123,
#26124),(#26125,#26126),(#26127,#26128),(#26129,#26130),(#26131,#26132),
(#26133,#26134),(#26135,#26136),(#26137,#26138),(#26139,#26140),(#26141,
#26142),(#26143,#26144),(#26145,#26146),(#26147,#26148),(#26149,#26150),
(#26151,#26152),(#26153,#26154),(#26155,#26156),(#26157,#26158),(#26159,
#26160),(#26161,#26162),(#26163,#26164),(#26165,#26166),(#26167,#26168),
(#26169,#26170),(#26171,#26172),(#26173,#26174),(#26175,#26176),(#26177,
#26178),(#26179,#26180),(#26181,#26182),(#26183,#26184)),.UNSPECIFIED.,
 .F.,.F.,.F.)
B_SPLINE_SURFACE_WITH_KNOTS((6,1,1,1,1,1,1,1,1,1,1,1,1,1,1,1,1,1,1,1,1,
1,1,1,1,1,1,1,1,1,1,1,1,1,1,1,1,1,1,1,1,1,1,1,1,1,1,1,1,1,1,1,1,1,1,1,1,
1,1,1,1,1,1,1,1,6),(2,2),(-1.,-0.984615384615383,-0.969230769230768,-0.953846153846152,
-0.938461538461537,-0.923076923076922,-0.907692307692306,-0.892307692307691,
-0.876923076923076,-0.86153846153846,-0.846153846153845,-0.83076923076923,
-0.815384615384614,-0.799999999999999,-0.784615384615384,-0.769230769230768,
-0.753846153846153,-0.738461538461538,-0.723076923076922,-0.707692307692307,
-0.692307692307692,-0.676923076923076,-0.661538461538461,-0.646153846153846,
-0.63076923076923,-0.615384615384615,-0.6,-0.584615384615384,-0.569230769230769,
-0.553846153846154,-0.538461538461538,-0.523076923076923,-0.507692307692308,
-0.492307692307692,-0.476923076923077,-0.461538461538462,-0.446153846153846,
-0.430769230769231,-0.415384615384615,-0.4,-0.384615384615385,-0.369230769230769,
-0.353846153846154,-0.338461538461538,-0.323076923076923,-0.307692307692308,
-0.292307692307692,-0.276923076923077,-0.261538461538462,-0.246153846153846,
-0.230769230769231,-0.215384615384615,-0.2,-0.184615384615385,-0.169230769230769,
-0.153846153846154,-0.138461538461538,-0.123076923076923,-0.107692307692308,
-0.0923076923076923,-0.0769230769230769,-0.0615384615384615,-0.0461538461538462,
-0.0307692307692308,-0.0153846153846154,0.),(-1.,1.),.UNSPECIFIED.)
GEOMETRIC_REPRESENTATION_ITEM()
RATIONAL_B_SPLINE_SURFACE(((1.,1.),(1.,1.),(1.,1.),(1.,1.),(1.,1.),(1.,
1.),(1.,1.),(1.,1.),(1.,1.),(1.,1.),(1.,1.),(1.,1.),(1.,1.),(1.,1.),(1.,
1.),(1.,1.),(1.,1.),(1.,1.),(1.,1.),(1.,1.),(1.,1.),(1.,1.),(1.,1.),(1.,
1.),(1.,1.),(1.,1.),(1.,1.),(1.,1.),(1.,1.),(1.,1.),(1.,1.),(1.,1.),(1.,
1.),(1.,1.),(1.,1.),(1.,1.),(1.,1.),(1.,1.),(1.,1.),(1.,1.),(1.,1.),(1.,
1.),(1.,1.),(1.,1.),(1.,1.),(1.,1.),(1.,1.),(1.,1.),(1.,1.),(1.,1.),(1.,
1.),(1.,1.),(1.,1.),(1.,1.),(1.,1.),(1.,1.),(1.,1.),(1.,1.),(1.,1.),(1.,
1.),(1.,1.),(1.,1.),(1.,1.),(1.,1.),(1.,1.),(1.,1.),(1.,1.),(1.,1.),(1.,
1.),(1.,1.)))
REPRESENTATION_ITEM('')
SURFACE()
);
#20=(
BOUNDED_SURFACE()
B_SPLINE_SURFACE(5,1,((#26261,#26262),(#26263,#26264),(#26265,#26266),(#26267,
#26268),(#26269,#26270),(#26271,#26272),(#26273,#26274),(#26275,#26276),
(#26277,#26278),(#26279,#26280),(#26281,#26282),(#26283,#26284),(#26285,
#26286),(#26287,#26288),(#26289,#26290),(#26291,#26292),(#26293,#26294),
(#26295,#26296),(#26297,#26298),(#26299,#26300),(#26301,#26302),(#26303,
#26304),(#26305,#26306),(#26307,#26308),(#26309,#26310),(#26311,#26312),
(#26313,#26314),(#26315,#26316),(#26317,#26318),(#26319,#26320),(#26321,
#26322),(#26323,#26324),(#26325,#26326),(#26327,#26328),(#26329,#26330),
(#26331,#26332),(#26333,#26334),(#26335,#26336),(#26337,#26338),(#26339,
#26340),(#26341,#26342),(#26343,#26344),(#26345,#26346),(#26347,#26348),
(#26349,#26350),(#26351,#26352),(#26353,#26354),(#26355,#26356),(#26357,
#26358),(#26359,#26360),(#26361,#26362),(#26363,#26364),(#26365,#26366),
(#26367,#26368),(#26369,#26370),(#26371,#26372),(#26373,#26374),(#26375,
#26376),(#26377,#26378),(#26379,#26380),(#26381,#26382),(#26383,#26384),
(#26385,#26386),(#26387,#26388),(#26389,#26390),(#26391,#26392),(#26393,
#26394),(#26395,#26396),(#26397,#26398),(#26399,#26400)),.UNSPECIFIED.,
 .F.,.F.,.F.)
B_SPLINE_SURFACE_WITH_KNOTS((6,1,1,1,1,1,1,1,1,1,1,1,1,1,1,1,1,1,1,1,1,
1,1,1,1,1,1,1,1,1,1,1,1,1,1,1,1,1,1,1,1,1,1,1,1,1,1,1,1,1,1,1,1,1,1,1,1,
1,1,1,1,1,1,1,1,6),(2,2),(-1.,-0.984615384615383,-0.969230769230768,-0.953846153846152,
-0.938461538461537,-0.923076923076922,-0.907692307692306,-0.892307692307691,
-0.876923076923076,-0.86153846153846,-0.846153846153845,-0.83076923076923,
-0.815384615384614,-0.799999999999999,-0.784615384615384,-0.769230769230768,
-0.753846153846153,-0.738461538461538,-0.723076923076922,-0.707692307692307,
-0.692307692307692,-0.676923076923076,-0.661538461538461,-0.646153846153846,
-0.63076923076923,-0.615384615384615,-0.6,-0.584615384615384,-0.569230769230769,
-0.553846153846154,-0.538461538461538,-0.523076923076923,-0.507692307692308,
-0.492307692307692,-0.476923076923077,-0.461538461538462,-0.446153846153846,
-0.430769230769231,-0.415384615384615,-0.4,-0.384615384615385,-0.369230769230769,
-0.353846153846154,-0.338461538461538,-0.323076923076923,-0.307692307692308,
-0.292307692307692,-0.276923076923077,-0.261538461538462,-0.246153846153846,
-0.230769230769231,-0.215384615384615,-0.2,-0.184615384615385,-0.169230769230769,
-0.153846153846154,-0.138461538461538,-0.123076923076923,-0.107692307692308,
-0.0923076923076923,-0.0769230769230769,-0.0615384615384615,-0.0461538461538462,
-0.0307692307692308,-0.0153846153846154,0.),(-1.,1.),.UNSPECIFIED.)
GEOMETRIC_REPRESENTATION_ITEM()
RATIONAL_B_SPLINE_SURFACE(((1.,1.),(1.,1.),(1.,1.),(1.,1.),(1.,1.),(1.,
1.),(1.,1.),(1.,1.),(1.,1.),(1.,1.),(1.,1.),(1.,1.),(1.,1.),(1.,1.),(1.,
1.),(1.,1.),(1.,1.),(1.,1.),(1.,1.),(1.,1.),(1.,1.),(1.,1.),(1.,1.),(1.,
1.),(1.,1.),(1.,1.),(1.,1.),(1.,1.),(1.,1.),(1.,1.),(1.,1.),(1.,1.),(1.,
1.),(1.,1.),(1.,1.),(1.,1.),(1.,1.),(1.,1.),(1.,1.),(1.,1.),(1.,1.),(1.,
1.),(1.,1.),(1.,1.),(1.,1.),(1.,1.),(1.,1.),(1.,1.),(1.,1.),(1.,1.),(1.,
1.),(1.,1.),(1.,1.),(1.,1.),(1.,1.),(1.,1.),(1.,1.),(1.,1.),(1.,1.),(1.,
1.),(1.,1.),(1.,1.),(1.,1.),(1.,1.),(1.,1.),(1.,1.),(1.,1.),(1.,1.),(1.,
1.),(1.,1.)))
REPRESENTATION_ITEM('')
SURFACE()
);
#21=(
BOUNDED_SURFACE()
B_SPLINE_SURFACE(5,1,((#26477,#26478),(#26479,#26480),(#26481,#26482),(#26483,
#26484),(#26485,#26486),(#26487,#26488),(#26489,#26490),(#26491,#26492),
(#26493,#26494),(#26495,#26496),(#26497,#26498),(#26499,#26500),(#26501,
#26502),(#26503,#26504),(#26505,#26506),(#26507,#26508),(#26509,#26510),
(#26511,#26512),(#26513,#26514),(#26515,#26516),(#26517,#26518),(#26519,
#26520),(#26521,#26522),(#26523,#26524),(#26525,#26526),(#26527,#26528),
(#26529,#26530),(#26531,#26532),(#26533,#26534),(#26535,#26536),(#26537,
#26538),(#26539,#26540),(#26541,#26542),(#26543,#26544),(#26545,#26546),
(#26547,#26548),(#26549,#26550),(#26551,#26552),(#26553,#26554),(#26555,
#26556),(#26557,#26558),(#26559,#26560),(#26561,#26562),(#26563,#26564),
(#26565,#26566),(#26567,#26568),(#26569,#26570),(#26571,#26572),(#26573,
#26574),(#26575,#26576),(#26577,#26578),(#26579,#26580),(#26581,#26582),
(#26583,#26584),(#26585,#26586),(#26587,#26588),(#26589,#26590),(#26591,
#26592),(#26593,#26594),(#26595,#26596),(#26597,#26598),(#26599,#26600),
(#26601,#26602),(#26603,#26604),(#26605,#26606),(#26607,#26608),(#26609,
#26610),(#26611,#26612),(#26613,#26614),(#26615,#26616)),.UNSPECIFIED.,
 .F.,.F.,.F.)
B_SPLINE_SURFACE_WITH_KNOTS((6,1,1,1,1,1,1,1,1,1,1,1,1,1,1,1,1,1,1,1,1,
1,1,1,1,1,1,1,1,1,1,1,1,1,1,1,1,1,1,1,1,1,1,1,1,1,1,1,1,1,1,1,1,1,1,1,1,
1,1,1,1,1,1,1,1,6),(2,2),(-1.,-0.984615384615383,-0.969230769230768,-0.953846153846152,
-0.938461538461537,-0.923076923076922,-0.907692307692306,-0.892307692307691,
-0.876923076923076,-0.86153846153846,-0.846153846153845,-0.83076923076923,
-0.815384615384614,-0.799999999999999,-0.784615384615384,-0.769230769230768,
-0.753846153846153,-0.738461538461538,-0.723076923076922,-0.707692307692307,
-0.692307692307692,-0.676923076923076,-0.661538461538461,-0.646153846153846,
-0.63076923076923,-0.615384615384615,-0.6,-0.584615384615384,-0.569230769230769,
-0.553846153846154,-0.538461538461538,-0.523076923076923,-0.507692307692308,
-0.492307692307692,-0.476923076923077,-0.461538461538462,-0.446153846153846,
-0.430769230769231,-0.415384615384615,-0.4,-0.384615384615385,-0.369230769230769,
-0.353846153846154,-0.338461538461538,-0.323076923076923,-0.307692307692308,
-0.292307692307692,-0.276923076923077,-0.261538461538462,-0.246153846153846,
-0.230769230769231,-0.215384615384615,-0.2,-0.184615384615385,-0.169230769230769,
-0.153846153846154,-0.138461538461538,-0.123076923076923,-0.107692307692308,
-0.0923076923076923,-0.0769230769230769,-0.0615384615384615,-0.0461538461538462,
-0.0307692307692308,-0.0153846153846154,0.),(-1.,1.),.UNSPECIFIED.)
GEOMETRIC_REPRESENTATION_ITEM()
RATIONAL_B_SPLINE_SURFACE(((1.,1.),(1.,1.),(1.,1.),(1.,1.),(1.,1.),(1.,
1.),(1.,1.),(1.,1.),(1.,1.),(1.,1.),(1.,1.),(1.,1.),(1.,1.),(1.,1.),(1.,
1.),(1.,1.),(1.,1.),(1.,1.),(1.,1.),(1.,1.),(1.,1.),(1.,1.),(1.,1.),(1.,
1.),(1.,1.),(1.,1.),(1.,1.),(1.,1.),(1.,1.),(1.,1.),(1.,1.),(1.,1.),(1.,
1.),(1.,1.),(1.,1.),(1.,1.),(1.,1.),(1.,1.),(1.,1.),(1.,1.),(1.,1.),(1.,
1.),(1.,1.),(1.,1.),(1.,1.),(1.,1.),(1.,1.),(1.,1.),(1.,1.),(1.,1.),(1.,
1.),(1.,1.),(1.,1.),(1.,1.),(1.,1.),(1.,1.),(1.,1.),(1.,1.),(1.,1.),(1.,
1.),(1.,1.),(1.,1.),(1.,1.),(1.,1.),(1.,1.),(1.,1.),(1.,1.),(1.,1.),(1.,
1.),(1.,1.)))
REPRESENTATION_ITEM('')
SURFACE()
);
#22=(
BOUNDED_SURFACE()
B_SPLINE_SURFACE(5,1,((#26693,#26694),(#26695,#26696),(#26697,#26698),(#26699,
#26700),(#26701,#26702),(#26703,#26704),(#26705,#26706),(#26707,#26708),
(#26709,#26710),(#26711,#26712),(#26713,#26714),(#26715,#26716),(#26717,
#26718),(#26719,#26720),(#26721,#26722),(#26723,#26724),(#26725,#26726),
(#26727,#26728),(#26729,#26730),(#26731,#26732),(#26733,#26734),(#26735,
#26736),(#26737,#26738),(#26739,#26740),(#26741,#26742),(#26743,#26744),
(#26745,#26746),(#26747,#26748),(#26749,#26750),(#26751,#26752),(#26753,
#26754),(#26755,#26756),(#26757,#26758),(#26759,#26760),(#26761,#26762),
(#26763,#26764),(#26765,#26766),(#26767,#26768),(#26769,#26770),(#26771,
#26772),(#26773,#26774),(#26775,#26776),(#26777,#26778),(#26779,#26780),
(#26781,#26782),(#26783,#26784),(#26785,#26786),(#26787,#26788),(#26789,
#26790),(#26791,#26792),(#26793,#26794),(#26795,#26796),(#26797,#26798),
(#26799,#26800),(#26801,#26802),(#26803,#26804),(#26805,#26806),(#26807,
#26808),(#26809,#26810),(#26811,#26812),(#26813,#26814),(#26815,#26816),
(#26817,#26818),(#26819,#26820),(#26821,#26822),(#26823,#26824),(#26825,
#26826),(#26827,#26828),(#26829,#26830),(#26831,#26832)),.UNSPECIFIED.,
 .F.,.F.,.F.)
B_SPLINE_SURFACE_WITH_KNOTS((6,1,1,1,1,1,1,1,1,1,1,1,1,1,1,1,1,1,1,1,1,
1,1,1,1,1,1,1,1,1,1,1,1,1,1,1,1,1,1,1,1,1,1,1,1,1,1,1,1,1,1,1,1,1,1,1,1,
1,1,1,1,1,1,1,1,6),(2,2),(-1.,-0.984615384615383,-0.969230769230768,-0.953846153846152,
-0.938461538461537,-0.923076923076922,-0.907692307692306,-0.892307692307691,
-0.876923076923076,-0.86153846153846,-0.846153846153845,-0.83076923076923,
-0.815384615384614,-0.799999999999999,-0.784615384615384,-0.769230769230768,
-0.753846153846153,-0.738461538461538,-0.723076923076922,-0.707692307692307,
-0.692307692307692,-0.676923076923076,-0.661538461538461,-0.646153846153846,
-0.63076923076923,-0.615384615384615,-0.6,-0.584615384615384,-0.569230769230769,
-0.553846153846154,-0.538461538461538,-0.523076923076923,-0.507692307692308,
-0.492307692307692,-0.476923076923077,-0.461538461538462,-0.446153846153846,
-0.430769230769231,-0.415384615384615,-0.4,-0.384615384615385,-0.369230769230769,
-0.353846153846154,-0.338461538461538,-0.323076923076923,-0.307692307692308,
-0.292307692307692,-0.276923076923077,-0.261538461538462,-0.246153846153846,
-0.230769230769231,-0.215384615384615,-0.2,-0.184615384615385,-0.169230769230769,
-0.153846153846154,-0.138461538461538,-0.123076923076923,-0.107692307692308,
-0.0923076923076923,-0.0769230769230769,-0.0615384615384615,-0.0461538461538462,
-0.0307692307692308,-0.0153846153846154,0.),(-1.,1.),.UNSPECIFIED.)
GEOMETRIC_REPRESENTATION_ITEM()
RATIONAL_B_SPLINE_SURFACE(((1.,1.),(1.,1.),(1.,1.),(1.,1.),(1.,1.),(1.,
1.),(1.,1.),(1.,1.),(1.,1.),(1.,1.),(1.,1.),(1.,1.),(1.,1.),(1.,1.),(1.,
1.),(1.,1.),(1.,1.),(1.,1.),(1.,1.),(1.,1.),(1.,1.),(1.,1.),(1.,1.),(1.,
1.),(1.,1.),(1.,1.),(1.,1.),(1.,1.),(1.,1.),(1.,1.),(1.,1.),(1.,1.),(1.,
1.),(1.,1.),(1.,1.),(1.,1.),(1.,1.),(1.,1.),(1.,1.),(1.,1.),(1.,1.),(1.,
1.),(1.,1.),(1.,1.),(1.,1.),(1.,1.),(1.,1.),(1.,1.),(1.,1.),(1.,1.),(1.,
1.),(1.,1.),(1.,1.),(1.,1.),(1.,1.),(1.,1.),(1.,1.),(1.,1.),(1.,1.),(1.,
1.),(1.,1.),(1.,1.),(1.,1.),(1.,1.),(1.,1.),(1.,1.),(1.,1.),(1.,1.),(1.,
1.),(1.,1.)))
REPRESENTATION_ITEM('')
SURFACE()
);
#23=(
BOUNDED_SURFACE()
B_SPLINE_SURFACE(5,1,((#26909,#26910),(#26911,#26912),(#26913,#26914),(#26915,
#26916),(#26917,#26918),(#26919,#26920),(#26921,#26922),(#26923,#26924),
(#26925,#26926),(#26927,#26928),(#26929,#26930),(#26931,#26932),(#26933,
#26934),(#26935,#26936),(#26937,#26938),(#26939,#26940),(#26941,#26942),
(#26943,#26944),(#26945,#26946),(#26947,#26948),(#26949,#26950),(#26951,
#26952),(#26953,#26954),(#26955,#26956),(#26957,#26958),(#26959,#26960),
(#26961,#26962),(#26963,#26964),(#26965,#26966),(#26967,#26968),(#26969,
#26970),(#26971,#26972),(#26973,#26974),(#26975,#26976),(#26977,#26978),
(#26979,#26980),(#26981,#26982),(#26983,#26984),(#26985,#26986),(#26987,
#26988),(#26989,#26990),(#26991,#26992),(#26993,#26994),(#26995,#26996),
(#26997,#26998),(#26999,#27000),(#27001,#27002),(#27003,#27004),(#27005,
#27006),(#27007,#27008),(#27009,#27010),(#27011,#27012),(#27013,#27014),
(#27015,#27016),(#27017,#27018),(#27019,#27020),(#27021,#27022),(#27023,
#27024),(#27025,#27026),(#27027,#27028),(#27029,#27030),(#27031,#27032),
(#27033,#27034),(#27035,#27036),(#27037,#27038),(#27039,#27040),(#27041,
#27042),(#27043,#27044),(#27045,#27046),(#27047,#27048)),.UNSPECIFIED.,
 .F.,.F.,.F.)
B_SPLINE_SURFACE_WITH_KNOTS((6,1,1,1,1,1,1,1,1,1,1,1,1,1,1,1,1,1,1,1,1,
1,1,1,1,1,1,1,1,1,1,1,1,1,1,1,1,1,1,1,1,1,1,1,1,1,1,1,1,1,1,1,1,1,1,1,1,
1,1,1,1,1,1,1,1,6),(2,2),(-1.,-0.984615384615383,-0.969230769230768,-0.953846153846152,
-0.938461538461537,-0.923076923076922,-0.907692307692306,-0.892307692307691,
-0.876923076923076,-0.86153846153846,-0.846153846153845,-0.83076923076923,
-0.815384615384614,-0.799999999999999,-0.784615384615384,-0.769230769230768,
-0.753846153846153,-0.738461538461538,-0.723076923076922,-0.707692307692307,
-0.692307692307692,-0.676923076923076,-0.661538461538461,-0.646153846153846,
-0.63076923076923,-0.615384615384615,-0.6,-0.584615384615384,-0.569230769230769,
-0.553846153846154,-0.538461538461538,-0.523076923076923,-0.507692307692308,
-0.492307692307692,-0.476923076923077,-0.461538461538462,-0.446153846153846,
-0.430769230769231,-0.415384615384615,-0.4,-0.384615384615385,-0.369230769230769,
-0.353846153846154,-0.338461538461538,-0.323076923076923,-0.307692307692308,
-0.292307692307692,-0.276923076923077,-0.261538461538462,-0.246153846153846,
-0.230769230769231,-0.215384615384615,-0.2,-0.184615384615385,-0.169230769230769,
-0.153846153846154,-0.138461538461538,-0.123076923076923,-0.107692307692308,
-0.0923076923076923,-0.0769230769230769,-0.0615384615384615,-0.0461538461538462,
-0.0307692307692308,-0.0153846153846154,0.),(-1.,1.),.UNSPECIFIED.)
GEOMETRIC_REPRESENTATION_ITEM()
RATIONAL_B_SPLINE_SURFACE(((1.,1.),(1.,1.),(1.,1.),(1.,1.),(1.,1.),(1.,
1.),(1.,1.),(1.,1.),(1.,1.),(1.,1.),(1.,1.),(1.,1.),(1.,1.),(1.,1.),(1.,
1.),(1.,1.),(1.,1.),(1.,1.),(1.,1.),(1.,1.),(1.,1.),(1.,1.),(1.,1.),(1.,
1.),(1.,1.),(1.,1.),(1.,1.),(1.,1.),(1.,1.),(1.,1.),(1.,1.),(1.,1.),(1.,
1.),(1.,1.),(1.,1.),(1.,1.),(1.,1.),(1.,1.),(1.,1.),(1.,1.),(1.,1.),(1.,
1.),(1.,1.),(1.,1.),(1.,1.),(1.,1.),(1.,1.),(1.,1.),(1.,1.),(1.,1.),(1.,
1.),(1.,1.),(1.,1.),(1.,1.),(1.,1.),(1.,1.),(1.,1.),(1.,1.),(1.,1.),(1.,
1.),(1.,1.),(1.,1.),(1.,1.),(1.,1.),(1.,1.),(1.,1.),(1.,1.),(1.,1.),(1.,
1.),(1.,1.)))
REPRESENTATION_ITEM('')
SURFACE()
);
#24=(
BOUNDED_SURFACE()
B_SPLINE_SURFACE(5,1,((#27125,#27126),(#27127,#27128),(#27129,#27130),(#27131,
#27132),(#27133,#27134),(#27135,#27136),(#27137,#27138),(#27139,#27140),
(#27141,#27142),(#27143,#27144),(#27145,#27146),(#27147,#27148),(#27149,
#27150),(#27151,#27152),(#27153,#27154),(#27155,#27156),(#27157,#27158),
(#27159,#27160),(#27161,#27162),(#27163,#27164),(#27165,#27166),(#27167,
#27168),(#27169,#27170),(#27171,#27172),(#27173,#27174),(#27175,#27176),
(#27177,#27178),(#27179,#27180),(#27181,#27182),(#27183,#27184),(#27185,
#27186),(#27187,#27188),(#27189,#27190),(#27191,#27192),(#27193,#27194),
(#27195,#27196),(#27197,#27198),(#27199,#27200),(#27201,#27202),(#27203,
#27204),(#27205,#27206),(#27207,#27208),(#27209,#27210),(#27211,#27212),
(#27213,#27214),(#27215,#27216),(#27217,#27218),(#27219,#27220),(#27221,
#27222),(#27223,#27224),(#27225,#27226),(#27227,#27228),(#27229,#27230),
(#27231,#27232),(#27233,#27234),(#27235,#27236),(#27237,#27238),(#27239,
#27240),(#27241,#27242),(#27243,#27244),(#27245,#27246),(#27247,#27248),
(#27249,#27250),(#27251,#27252),(#27253,#27254),(#27255,#27256),(#27257,
#27258),(#27259,#27260),(#27261,#27262),(#27263,#27264)),.UNSPECIFIED.,
 .F.,.F.,.F.)
B_SPLINE_SURFACE_WITH_KNOTS((6,1,1,1,1,1,1,1,1,1,1,1,1,1,1,1,1,1,1,1,1,
1,1,1,1,1,1,1,1,1,1,1,1,1,1,1,1,1,1,1,1,1,1,1,1,1,1,1,1,1,1,1,1,1,1,1,1,
1,1,1,1,1,1,1,1,6),(2,2),(-1.,-0.984615384615383,-0.969230769230768,-0.953846153846152,
-0.938461538461537,-0.923076923076922,-0.907692307692306,-0.892307692307691,
-0.876923076923076,-0.86153846153846,-0.846153846153845,-0.83076923076923,
-0.815384615384614,-0.799999999999999,-0.784615384615384,-0.769230769230768,
-0.753846153846153,-0.738461538461538,-0.723076923076922,-0.707692307692307,
-0.692307692307692,-0.676923076923076,-0.661538461538461,-0.646153846153846,
-0.63076923076923,-0.615384615384615,-0.6,-0.584615384615384,-0.569230769230769,
-0.553846153846154,-0.538461538461538,-0.523076923076923,-0.507692307692308,
-0.492307692307692,-0.476923076923077,-0.461538461538462,-0.446153846153846,
-0.430769230769231,-0.415384615384615,-0.4,-0.384615384615385,-0.369230769230769,
-0.353846153846154,-0.338461538461538,-0.323076923076923,-0.307692307692308,
-0.292307692307692,-0.276923076923077,-0.261538461538462,-0.246153846153846,
-0.230769230769231,-0.215384615384615,-0.2,-0.184615384615385,-0.169230769230769,
-0.153846153846154,-0.138461538461538,-0.123076923076923,-0.107692307692308,
-0.0923076923076923,-0.0769230769230769,-0.0615384615384615,-0.0461538461538462,
-0.0307692307692308,-0.0153846153846154,0.),(-1.,1.),.UNSPECIFIED.)
GEOMETRIC_REPRESENTATION_ITEM()
RATIONAL_B_SPLINE_SURFACE(((1.,1.),(1.,1.),(1.,1.),(1.,1.),(1.,1.),(1.,
1.),(1.,1.),(1.,1.),(1.,1.),(1.,1.),(1.,1.),(1.,1.),(1.,1.),(1.,1.),(1.,
1.),(1.,1.),(1.,1.),(1.,1.),(1.,1.),(1.,1.),(1.,1.),(1.,1.),(1.,1.),(1.,
1.),(1.,1.),(1.,1.),(1.,1.),(1.,1.),(1.,1.),(1.,1.),(1.,1.),(1.,1.),(1.,
1.),(1.,1.),(1.,1.),(1.,1.),(1.,1.),(1.,1.),(1.,1.),(1.,1.),(1.,1.),(1.,
1.),(1.,1.),(1.,1.),(1.,1.),(1.,1.),(1.,1.),(1.,1.),(1.,1.),(1.,1.),(1.,
1.),(1.,1.),(1.,1.),(1.,1.),(1.,1.),(1.,1.),(1.,1.),(1.,1.),(1.,1.),(1.,
1.),(1.,1.),(1.,1.),(1.,1.),(1.,1.),(1.,1.),(1.,1.),(1.,1.),(1.,1.),(1.,
1.),(1.,1.)))
REPRESENTATION_ITEM('')
SURFACE()
);
#25=(
BOUNDED_SURFACE()
B_SPLINE_SURFACE(5,1,((#27341,#27342),(#27343,#27344),(#27345,#27346),(#27347,
#27348),(#27349,#27350),(#27351,#27352),(#27353,#27354),(#27355,#27356),
(#27357,#27358),(#27359,#27360),(#27361,#27362),(#27363,#27364),(#27365,
#27366),(#27367,#27368),(#27369,#27370),(#27371,#27372),(#27373,#27374),
(#27375,#27376),(#27377,#27378),(#27379,#27380),(#27381,#27382),(#27383,
#27384),(#27385,#27386),(#27387,#27388),(#27389,#27390),(#27391,#27392),
(#27393,#27394),(#27395,#27396),(#27397,#27398),(#27399,#27400),(#27401,
#27402),(#27403,#27404),(#27405,#27406),(#27407,#27408),(#27409,#27410),
(#27411,#27412),(#27413,#27414),(#27415,#27416),(#27417,#27418),(#27419,
#27420),(#27421,#27422),(#27423,#27424),(#27425,#27426),(#27427,#27428),
(#27429,#27430),(#27431,#27432),(#27433,#27434),(#27435,#27436),(#27437,
#27438),(#27439,#27440),(#27441,#27442),(#27443,#27444),(#27445,#27446),
(#27447,#27448),(#27449,#27450),(#27451,#27452),(#27453,#27454),(#27455,
#27456),(#27457,#27458),(#27459,#27460),(#27461,#27462),(#27463,#27464),
(#27465,#27466),(#27467,#27468),(#27469,#27470),(#27471,#27472),(#27473,
#27474),(#27475,#27476),(#27477,#27478),(#27479,#27480)),.UNSPECIFIED.,
 .F.,.F.,.F.)
B_SPLINE_SURFACE_WITH_KNOTS((6,1,1,1,1,1,1,1,1,1,1,1,1,1,1,1,1,1,1,1,1,
1,1,1,1,1,1,1,1,1,1,1,1,1,1,1,1,1,1,1,1,1,1,1,1,1,1,1,1,1,1,1,1,1,1,1,1,
1,1,1,1,1,1,1,1,6),(2,2),(-1.,-0.984615384615383,-0.969230769230768,-0.953846153846152,
-0.938461538461537,-0.923076923076922,-0.907692307692306,-0.892307692307691,
-0.876923076923076,-0.86153846153846,-0.846153846153845,-0.83076923076923,
-0.815384615384614,-0.799999999999999,-0.784615384615384,-0.769230769230768,
-0.753846153846153,-0.738461538461538,-0.723076923076922,-0.707692307692307,
-0.692307692307692,-0.676923076923076,-0.661538461538461,-0.646153846153846,
-0.63076923076923,-0.615384615384615,-0.6,-0.584615384615384,-0.569230769230769,
-0.553846153846154,-0.538461538461538,-0.523076923076923,-0.507692307692308,
-0.492307692307692,-0.476923076923077,-0.461538461538462,-0.446153846153846,
-0.430769230769231,-0.415384615384615,-0.4,-0.384615384615385,-0.369230769230769,
-0.353846153846154,-0.338461538461538,-0.323076923076923,-0.307692307692308,
-0.292307692307692,-0.276923076923077,-0.261538461538462,-0.246153846153846,
-0.230769230769231,-0.215384615384615,-0.2,-0.184615384615385,-0.169230769230769,
-0.153846153846154,-0.138461538461538,-0.123076923076923,-0.107692307692308,
-0.0923076923076923,-0.0769230769230769,-0.0615384615384615,-0.0461538461538462,
-0.0307692307692308,-0.0153846153846154,0.),(-1.,1.),.UNSPECIFIED.)
GEOMETRIC_REPRESENTATION_ITEM()
RATIONAL_B_SPLINE_SURFACE(((1.,1.),(1.,1.),(1.,1.),(1.,1.),(1.,1.),(1.,
1.),(1.,1.),(1.,1.),(1.,1.),(1.,1.),(1.,1.),(1.,1.),(1.,1.),(1.,1.),(1.,
1.),(1.,1.),(1.,1.),(1.,1.),(1.,1.),(1.,1.),(1.,1.),(1.,1.),(1.,1.),(1.,
1.),(1.,1.),(1.,1.),(1.,1.),(1.,1.),(1.,1.),(1.,1.),(1.,1.),(1.,1.),(1.,
1.),(1.,1.),(1.,1.),(1.,1.),(1.,1.),(1.,1.),(1.,1.),(1.,1.),(1.,1.),(1.,
1.),(1.,1.),(1.,1.),(1.,1.),(1.,1.),(1.,1.),(1.,1.),(1.,1.),(1.,1.),(1.,
1.),(1.,1.),(1.,1.),(1.,1.),(1.,1.),(1.,1.),(1.,1.),(1.,1.),(1.,1.),(1.,
1.),(1.,1.),(1.,1.),(1.,1.),(1.,1.),(1.,1.),(1.,1.),(1.,1.),(1.,1.),(1.,
1.),(1.,1.)))
REPRESENTATION_ITEM('')
SURFACE()
);
#26=(
BOUNDED_SURFACE()
B_SPLINE_SURFACE(5,1,((#27557,#27558),(#27559,#27560),(#27561,#27562),(#27563,
#27564),(#27565,#27566),(#27567,#27568),(#27569,#27570),(#27571,#27572),
(#27573,#27574),(#27575,#27576),(#27577,#27578),(#27579,#27580),(#27581,
#27582),(#27583,#27584),(#27585,#27586),(#27587,#27588),(#27589,#27590),
(#27591,#27592),(#27593,#27594),(#27595,#27596),(#27597,#27598),(#27599,
#27600),(#27601,#27602),(#27603,#27604),(#27605,#27606),(#27607,#27608),
(#27609,#27610),(#27611,#27612),(#27613,#27614),(#27615,#27616),(#27617,
#27618),(#27619,#27620),(#27621,#27622),(#27623,#27624),(#27625,#27626),
(#27627,#27628),(#27629,#27630),(#27631,#27632),(#27633,#27634),(#27635,
#27636),(#27637,#27638),(#27639,#27640),(#27641,#27642),(#27643,#27644),
(#27645,#27646),(#27647,#27648),(#27649,#27650),(#27651,#27652),(#27653,
#27654),(#27655,#27656),(#27657,#27658),(#27659,#27660),(#27661,#27662),
(#27663,#27664),(#27665,#27666),(#27667,#27668),(#27669,#27670),(#27671,
#27672),(#27673,#27674),(#27675,#27676),(#27677,#27678),(#27679,#27680),
(#27681,#27682),(#27683,#27684),(#27685,#27686),(#27687,#27688),(#27689,
#27690),(#27691,#27692),(#27693,#27694),(#27695,#27696)),.UNSPECIFIED.,
 .F.,.F.,.F.)
B_SPLINE_SURFACE_WITH_KNOTS((6,1,1,1,1,1,1,1,1,1,1,1,1,1,1,1,1,1,1,1,1,
1,1,1,1,1,1,1,1,1,1,1,1,1,1,1,1,1,1,1,1,1,1,1,1,1,1,1,1,1,1,1,1,1,1,1,1,
1,1,1,1,1,1,1,1,6),(2,2),(-1.,-0.984615384615383,-0.969230769230768,-0.953846153846152,
-0.938461538461537,-0.923076923076922,-0.907692307692306,-0.892307692307691,
-0.876923076923076,-0.86153846153846,-0.846153846153845,-0.83076923076923,
-0.815384615384614,-0.799999999999999,-0.784615384615384,-0.769230769230768,
-0.753846153846153,-0.738461538461538,-0.723076923076922,-0.707692307692307,
-0.692307692307692,-0.676923076923076,-0.661538461538461,-0.646153846153846,
-0.63076923076923,-0.615384615384615,-0.6,-0.584615384615384,-0.569230769230769,
-0.553846153846154,-0.538461538461538,-0.523076923076923,-0.507692307692308,
-0.492307692307692,-0.476923076923077,-0.461538461538462,-0.446153846153846,
-0.430769230769231,-0.415384615384615,-0.4,-0.384615384615385,-0.369230769230769,
-0.353846153846154,-0.338461538461538,-0.323076923076923,-0.307692307692308,
-0.292307692307692,-0.276923076923077,-0.261538461538462,-0.246153846153846,
-0.230769230769231,-0.215384615384615,-0.2,-0.184615384615385,-0.169230769230769,
-0.153846153846154,-0.138461538461538,-0.123076923076923,-0.107692307692308,
-0.0923076923076923,-0.0769230769230769,-0.0615384615384615,-0.0461538461538462,
-0.0307692307692308,-0.0153846153846154,0.),(-1.,1.),.UNSPECIFIED.)
GEOMETRIC_REPRESENTATION_ITEM()
RATIONAL_B_SPLINE_SURFACE(((1.,1.),(1.,1.),(1.,1.),(1.,1.),(1.,1.),(1.,
1.),(1.,1.),(1.,1.),(1.,1.),(1.,1.),(1.,1.),(1.,1.),(1.,1.),(1.,1.),(1.,
1.),(1.,1.),(1.,1.),(1.,1.),(1.,1.),(1.,1.),(1.,1.),(1.,1.),(1.,1.),(1.,
1.),(1.,1.),(1.,1.),(1.,1.),(1.,1.),(1.,1.),(1.,1.),(1.,1.),(1.,1.),(1.,
1.),(1.,1.),(1.,1.),(1.,1.),(1.,1.),(1.,1.),(1.,1.),(1.,1.),(1.,1.),(1.,
1.),(1.,1.),(1.,1.),(1.,1.),(1.,1.),(1.,1.),(1.,1.),(1.,1.),(1.,1.),(1.,
1.),(1.,1.),(1.,1.),(1.,1.),(1.,1.),(1.,1.),(1.,1.),(1.,1.),(1.,1.),(1.,
1.),(1.,1.),(1.,1.),(1.,1.),(1.,1.),(1.,1.),(1.,1.),(1.,1.),(1.,1.),(1.,
1.),(1.,1.)))
REPRESENTATION_ITEM('')
SURFACE()
);
#27=(
BOUNDED_SURFACE()
B_SPLINE_SURFACE(5,1,((#27773,#27774),(#27775,#27776),(#27777,#27778),(#27779,
#27780),(#27781,#27782),(#27783,#27784),(#27785,#27786),(#27787,#27788),
(#27789,#27790),(#27791,#27792),(#27793,#27794),(#27795,#27796),(#27797,
#27798),(#27799,#27800),(#27801,#27802),(#27803,#27804),(#27805,#27806),
(#27807,#27808),(#27809,#27810),(#27811,#27812),(#27813,#27814),(#27815,
#27816),(#27817,#27818),(#27819,#27820),(#27821,#27822),(#27823,#27824),
(#27825,#27826),(#27827,#27828),(#27829,#27830),(#27831,#27832),(#27833,
#27834),(#27835,#27836),(#27837,#27838),(#27839,#27840),(#27841,#27842),
(#27843,#27844),(#27845,#27846),(#27847,#27848),(#27849,#27850),(#27851,
#27852),(#27853,#27854),(#27855,#27856),(#27857,#27858),(#27859,#27860),
(#27861,#27862),(#27863,#27864),(#27865,#27866),(#27867,#27868),(#27869,
#27870),(#27871,#27872),(#27873,#27874),(#27875,#27876),(#27877,#27878),
(#27879,#27880),(#27881,#27882),(#27883,#27884),(#27885,#27886),(#27887,
#27888),(#27889,#27890),(#27891,#27892),(#27893,#27894),(#27895,#27896),
(#27897,#27898),(#27899,#27900),(#27901,#27902),(#27903,#27904),(#27905,
#27906),(#27907,#27908),(#27909,#27910),(#27911,#27912)),.UNSPECIFIED.,
 .F.,.F.,.F.)
B_SPLINE_SURFACE_WITH_KNOTS((6,1,1,1,1,1,1,1,1,1,1,1,1,1,1,1,1,1,1,1,1,
1,1,1,1,1,1,1,1,1,1,1,1,1,1,1,1,1,1,1,1,1,1,1,1,1,1,1,1,1,1,1,1,1,1,1,1,
1,1,1,1,1,1,1,1,6),(2,2),(-1.,-0.984615384615383,-0.969230769230768,-0.953846153846152,
-0.938461538461537,-0.923076923076922,-0.907692307692306,-0.892307692307691,
-0.876923076923076,-0.86153846153846,-0.846153846153845,-0.83076923076923,
-0.815384615384614,-0.799999999999999,-0.784615384615384,-0.769230769230768,
-0.753846153846153,-0.738461538461538,-0.723076923076922,-0.707692307692307,
-0.692307692307692,-0.676923076923076,-0.661538461538461,-0.646153846153846,
-0.63076923076923,-0.615384615384615,-0.6,-0.584615384615384,-0.569230769230769,
-0.553846153846154,-0.538461538461538,-0.523076923076923,-0.507692307692308,
-0.492307692307692,-0.476923076923077,-0.461538461538462,-0.446153846153846,
-0.430769230769231,-0.415384615384615,-0.4,-0.384615384615385,-0.369230769230769,
-0.353846153846154,-0.338461538461538,-0.323076923076923,-0.307692307692308,
-0.292307692307692,-0.276923076923077,-0.261538461538462,-0.246153846153846,
-0.230769230769231,-0.215384615384615,-0.2,-0.184615384615385,-0.169230769230769,
-0.153846153846154,-0.138461538461538,-0.123076923076923,-0.107692307692308,
-0.0923076923076923,-0.0769230769230769,-0.0615384615384615,-0.0461538461538462,
-0.0307692307692308,-0.0153846153846154,0.),(-1.,1.),.UNSPECIFIED.)
GEOMETRIC_REPRESENTATION_ITEM()
RATIONAL_B_SPLINE_SURFACE(((1.,1.),(1.,1.),(1.,1.),(1.,1.),(1.,1.),(1.,
1.),(1.,1.),(1.,1.),(1.,1.),(1.,1.),(1.,1.),(1.,1.),(1.,1.),(1.,1.),(1.,
1.),(1.,1.),(1.,1.),(1.,1.),(1.,1.),(1.,1.),(1.,1.),(1.,1.),(1.,1.),(1.,
1.),(1.,1.),(1.,1.),(1.,1.),(1.,1.),(1.,1.),(1.,1.),(1.,1.),(1.,1.),(1.,
1.),(1.,1.),(1.,1.),(1.,1.),(1.,1.),(1.,1.),(1.,1.),(1.,1.),(1.,1.),(1.,
1.),(1.,1.),(1.,1.),(1.,1.),(1.,1.),(1.,1.),(1.,1.),(1.,1.),(1.,1.),(1.,
1.),(1.,1.),(1.,1.),(1.,1.),(1.,1.),(1.,1.),(1.,1.),(1.,1.),(1.,1.),(1.,
1.),(1.,1.),(1.,1.),(1.,1.),(1.,1.),(1.,1.),(1.,1.),(1.,1.),(1.,1.),(1.,
1.),(1.,1.)))
REPRESENTATION_ITEM('')
SURFACE()
);
#28=(
BOUNDED_SURFACE()
B_SPLINE_SURFACE(5,1,((#27989,#27990),(#27991,#27992),(#27993,#27994),(#27995,
#27996),(#27997,#27998),(#27999,#28000),(#28001,#28002),(#28003,#28004),
(#28005,#28006),(#28007,#28008),(#28009,#28010),(#28011,#28012),(#28013,
#28014),(#28015,#28016),(#28017,#28018),(#28019,#28020),(#28021,#28022),
(#28023,#28024),(#28025,#28026),(#28027,#28028),(#28029,#28030),(#28031,
#28032),(#28033,#28034),(#28035,#28036),(#28037,#28038),(#28039,#28040),
(#28041,#28042),(#28043,#28044),(#28045,#28046),(#28047,#28048),(#28049,
#28050),(#28051,#28052),(#28053,#28054),(#28055,#28056),(#28057,#28058),
(#28059,#28060),(#28061,#28062),(#28063,#28064),(#28065,#28066),(#28067,
#28068),(#28069,#28070),(#28071,#28072),(#28073,#28074),(#28075,#28076),
(#28077,#28078),(#28079,#28080),(#28081,#28082),(#28083,#28084),(#28085,
#28086),(#28087,#28088),(#28089,#28090),(#28091,#28092),(#28093,#28094),
(#28095,#28096),(#28097,#28098),(#28099,#28100),(#28101,#28102),(#28103,
#28104),(#28105,#28106),(#28107,#28108),(#28109,#28110),(#28111,#28112),
(#28113,#28114),(#28115,#28116),(#28117,#28118),(#28119,#28120),(#28121,
#28122),(#28123,#28124),(#28125,#28126),(#28127,#28128)),.UNSPECIFIED.,
 .F.,.F.,.F.)
B_SPLINE_SURFACE_WITH_KNOTS((6,1,1,1,1,1,1,1,1,1,1,1,1,1,1,1,1,1,1,1,1,
1,1,1,1,1,1,1,1,1,1,1,1,1,1,1,1,1,1,1,1,1,1,1,1,1,1,1,1,1,1,1,1,1,1,1,1,
1,1,1,1,1,1,1,1,6),(2,2),(-1.,-0.984615384615383,-0.969230769230768,-0.953846153846152,
-0.938461538461537,-0.923076923076922,-0.907692307692306,-0.892307692307691,
-0.876923076923076,-0.86153846153846,-0.846153846153845,-0.83076923076923,
-0.815384615384614,-0.799999999999999,-0.784615384615384,-0.769230769230768,
-0.753846153846153,-0.738461538461538,-0.723076923076922,-0.707692307692307,
-0.692307692307692,-0.676923076923076,-0.661538461538461,-0.646153846153846,
-0.63076923076923,-0.615384615384615,-0.6,-0.584615384615384,-0.569230769230769,
-0.553846153846154,-0.538461538461538,-0.523076923076923,-0.507692307692308,
-0.492307692307692,-0.476923076923077,-0.461538461538462,-0.446153846153846,
-0.430769230769231,-0.415384615384615,-0.4,-0.384615384615385,-0.369230769230769,
-0.353846153846154,-0.338461538461538,-0.323076923076923,-0.307692307692308,
-0.292307692307692,-0.276923076923077,-0.261538461538462,-0.246153846153846,
-0.230769230769231,-0.215384615384615,-0.2,-0.184615384615385,-0.169230769230769,
-0.153846153846154,-0.138461538461538,-0.123076923076923,-0.107692307692308,
-0.0923076923076923,-0.0769230769230769,-0.0615384615384615,-0.0461538461538462,
-0.0307692307692308,-0.0153846153846154,0.),(-1.,1.),.UNSPECIFIED.)
GEOMETRIC_REPRESENTATION_ITEM()
RATIONAL_B_SPLINE_SURFACE(((1.,1.),(1.,1.),(1.,1.),(1.,1.),(1.,1.),(1.,
1.),(1.,1.),(1.,1.),(1.,1.),(1.,1.),(1.,1.),(1.,1.),(1.,1.),(1.,1.),(1.,
1.),(1.,1.),(1.,1.),(1.,1.),(1.,1.),(1.,1.),(1.,1.),(1.,1.),(1.,1.),(1.,
1.),(1.,1.),(1.,1.),(1.,1.),(1.,1.),(1.,1.),(1.,1.),(1.,1.),(1.,1.),(1.,
1.),(1.,1.),(1.,1.),(1.,1.),(1.,1.),(1.,1.),(1.,1.),(1.,1.),(1.,1.),(1.,
1.),(1.,1.),(1.,1.),(1.,1.),(1.,1.),(1.,1.),(1.,1.),(1.,1.),(1.,1.),(1.,
1.),(1.,1.),(1.,1.),(1.,1.),(1.,1.),(1.,1.),(1.,1.),(1.,1.),(1.,1.),(1.,
1.),(1.,1.),(1.,1.),(1.,1.),(1.,1.),(1.,1.),(1.,1.),(1.,1.),(1.,1.),(1.,
1.),(1.,1.)))
REPRESENTATION_ITEM('')
SURFACE()
);
#29=(
BOUNDED_SURFACE()
B_SPLINE_SURFACE(5,1,((#28205,#28206),(#28207,#28208),(#28209,#28210),(#28211,
#28212),(#28213,#28214),(#28215,#28216),(#28217,#28218),(#28219,#28220),
(#28221,#28222),(#28223,#28224),(#28225,#28226),(#28227,#28228),(#28229,
#28230),(#28231,#28232),(#28233,#28234),(#28235,#28236),(#28237,#28238),
(#28239,#28240),(#28241,#28242),(#28243,#28244),(#28245,#28246),(#28247,
#28248),(#28249,#28250),(#28251,#28252),(#28253,#28254),(#28255,#28256),
(#28257,#28258),(#28259,#28260),(#28261,#28262),(#28263,#28264),(#28265,
#28266),(#28267,#28268),(#28269,#28270),(#28271,#28272),(#28273,#28274),
(#28275,#28276),(#28277,#28278),(#28279,#28280),(#28281,#28282),(#28283,
#28284),(#28285,#28286),(#28287,#28288),(#28289,#28290),(#28291,#28292),
(#28293,#28294),(#28295,#28296),(#28297,#28298),(#28299,#28300),(#28301,
#28302),(#28303,#28304),(#28305,#28306),(#28307,#28308),(#28309,#28310),
(#28311,#28312),(#28313,#28314),(#28315,#28316),(#28317,#28318),(#28319,
#28320),(#28321,#28322),(#28323,#28324),(#28325,#28326),(#28327,#28328),
(#28329,#28330),(#28331,#28332),(#28333,#28334),(#28335,#28336),(#28337,
#28338),(#28339,#28340),(#28341,#28342),(#28343,#28344)),.UNSPECIFIED.,
 .F.,.F.,.F.)
B_SPLINE_SURFACE_WITH_KNOTS((6,1,1,1,1,1,1,1,1,1,1,1,1,1,1,1,1,1,1,1,1,
1,1,1,1,1,1,1,1,1,1,1,1,1,1,1,1,1,1,1,1,1,1,1,1,1,1,1,1,1,1,1,1,1,1,1,1,
1,1,1,1,1,1,1,1,6),(2,2),(-1.,-0.984615384615383,-0.969230769230768,-0.953846153846152,
-0.938461538461537,-0.923076923076922,-0.907692307692306,-0.892307692307691,
-0.876923076923076,-0.86153846153846,-0.846153846153845,-0.83076923076923,
-0.815384615384614,-0.799999999999999,-0.784615384615384,-0.769230769230768,
-0.753846153846153,-0.738461538461538,-0.723076923076922,-0.707692307692307,
-0.692307692307692,-0.676923076923076,-0.661538461538461,-0.646153846153846,
-0.63076923076923,-0.615384615384615,-0.6,-0.584615384615384,-0.569230769230769,
-0.553846153846154,-0.538461538461538,-0.523076923076923,-0.507692307692308,
-0.492307692307692,-0.476923076923077,-0.461538461538462,-0.446153846153846,
-0.430769230769231,-0.415384615384615,-0.4,-0.384615384615385,-0.369230769230769,
-0.353846153846154,-0.338461538461538,-0.323076923076923,-0.307692307692308,
-0.292307692307692,-0.276923076923077,-0.261538461538462,-0.246153846153846,
-0.230769230769231,-0.215384615384615,-0.2,-0.184615384615385,-0.169230769230769,
-0.153846153846154,-0.138461538461538,-0.123076923076923,-0.107692307692308,
-0.0923076923076923,-0.0769230769230769,-0.0615384615384615,-0.0461538461538462,
-0.0307692307692308,-0.0153846153846154,0.),(-1.,1.),.UNSPECIFIED.)
GEOMETRIC_REPRESENTATION_ITEM()
RATIONAL_B_SPLINE_SURFACE(((1.,1.),(1.,1.),(1.,1.),(1.,1.),(1.,1.),(1.,
1.),(1.,1.),(1.,1.),(1.,1.),(1.,1.),(1.,1.),(1.,1.),(1.,1.),(1.,1.),(1.,
1.),(1.,1.),(1.,1.),(1.,1.),(1.,1.),(1.,1.),(1.,1.),(1.,1.),(1.,1.),(1.,
1.),(1.,1.),(1.,1.),(1.,1.),(1.,1.),(1.,1.),(1.,1.),(1.,1.),(1.,1.),(1.,
1.),(1.,1.),(1.,1.),(1.,1.),(1.,1.),(1.,1.),(1.,1.),(1.,1.),(1.,1.),(1.,
1.),(1.,1.),(1.,1.),(1.,1.),(1.,1.),(1.,1.),(1.,1.),(1.,1.),(1.,1.),(1.,
1.),(1.,1.),(1.,1.),(1.,1.),(1.,1.),(1.,1.),(1.,1.),(1.,1.),(1.,1.),(1.,
1.),(1.,1.),(1.,1.),(1.,1.),(1.,1.),(1.,1.),(1.,1.),(1.,1.),(1.,1.),(1.,
1.),(1.,1.)))
REPRESENTATION_ITEM('')
SURFACE()
);
#30=(
BOUNDED_SURFACE()
B_SPLINE_SURFACE(5,1,((#28421,#28422),(#28423,#28424),(#28425,#28426),(#28427,
#28428),(#28429,#28430),(#28431,#28432),(#28433,#28434),(#28435,#28436),
(#28437,#28438),(#28439,#28440),(#28441,#28442),(#28443,#28444),(#28445,
#28446),(#28447,#28448),(#28449,#28450),(#28451,#28452),(#28453,#28454),
(#28455,#28456),(#28457,#28458),(#28459,#28460),(#28461,#28462),(#28463,
#28464),(#28465,#28466),(#28467,#28468),(#28469,#28470),(#28471,#28472),
(#28473,#28474),(#28475,#28476),(#28477,#28478),(#28479,#28480),(#28481,
#28482),(#28483,#28484),(#28485,#28486),(#28487,#28488),(#28489,#28490),
(#28491,#28492),(#28493,#28494),(#28495,#28496),(#28497,#28498),(#28499,
#28500),(#28501,#28502),(#28503,#28504),(#28505,#28506),(#28507,#28508),
(#28509,#28510),(#28511,#28512),(#28513,#28514),(#28515,#28516),(#28517,
#28518),(#28519,#28520),(#28521,#28522),(#28523,#28524),(#28525,#28526),
(#28527,#28528),(#28529,#28530),(#28531,#28532),(#28533,#28534),(#28535,
#28536),(#28537,#28538),(#28539,#28540),(#28541,#28542),(#28543,#28544),
(#28545,#28546),(#28547,#28548),(#28549,#28550),(#28551,#28552),(#28553,
#28554),(#28555,#28556),(#28557,#28558),(#28559,#28560)),.UNSPECIFIED.,
 .F.,.F.,.F.)
B_SPLINE_SURFACE_WITH_KNOTS((6,1,1,1,1,1,1,1,1,1,1,1,1,1,1,1,1,1,1,1,1,
1,1,1,1,1,1,1,1,1,1,1,1,1,1,1,1,1,1,1,1,1,1,1,1,1,1,1,1,1,1,1,1,1,1,1,1,
1,1,1,1,1,1,1,1,6),(2,2),(-1.,-0.984615384615383,-0.969230769230768,-0.953846153846152,
-0.938461538461537,-0.923076923076922,-0.907692307692306,-0.892307692307691,
-0.876923076923076,-0.86153846153846,-0.846153846153845,-0.83076923076923,
-0.815384615384614,-0.799999999999999,-0.784615384615384,-0.769230769230768,
-0.753846153846153,-0.738461538461538,-0.723076923076922,-0.707692307692307,
-0.692307692307692,-0.676923076923076,-0.661538461538461,-0.646153846153846,
-0.63076923076923,-0.615384615384615,-0.6,-0.584615384615384,-0.569230769230769,
-0.553846153846154,-0.538461538461538,-0.523076923076923,-0.507692307692308,
-0.492307692307692,-0.476923076923077,-0.461538461538462,-0.446153846153846,
-0.430769230769231,-0.415384615384615,-0.4,-0.384615384615385,-0.369230769230769,
-0.353846153846154,-0.338461538461538,-0.323076923076923,-0.307692307692308,
-0.292307692307692,-0.276923076923077,-0.261538461538462,-0.246153846153846,
-0.230769230769231,-0.215384615384615,-0.2,-0.184615384615385,-0.169230769230769,
-0.153846153846154,-0.138461538461538,-0.123076923076923,-0.107692307692308,
-0.0923076923076923,-0.0769230769230769,-0.0615384615384615,-0.0461538461538462,
-0.0307692307692308,-0.0153846153846154,0.),(-1.,1.),.UNSPECIFIED.)
GEOMETRIC_REPRESENTATION_ITEM()
RATIONAL_B_SPLINE_SURFACE(((1.,1.),(1.,1.),(1.,1.),(1.,1.),(1.,1.),(1.,
1.),(1.,1.),(1.,1.),(1.,1.),(1.,1.),(1.,1.),(1.,1.),(1.,1.),(1.,1.),(1.,
1.),(1.,1.),(1.,1.),(1.,1.),(1.,1.),(1.,1.),(1.,1.),(1.,1.),(1.,1.),(1.,
1.),(1.,1.),(1.,1.),(1.,1.),(1.,1.),(1.,1.),(1.,1.),(1.,1.),(1.,1.),(1.,
1.),(1.,1.),(1.,1.),(1.,1.),(1.,1.),(1.,1.),(1.,1.),(1.,1.),(1.,1.),(1.,
1.),(1.,1.),(1.,1.),(1.,1.),(1.,1.),(1.,1.),(1.,1.),(1.,1.),(1.,1.),(1.,
1.),(1.,1.),(1.,1.),(1.,1.),(1.,1.),(1.,1.),(1.,1.),(1.,1.),(1.,1.),(1.,
1.),(1.,1.),(1.,1.),(1.,1.),(1.,1.),(1.,1.),(1.,1.),(1.,1.),(1.,1.),(1.,
1.),(1.,1.)))
REPRESENTATION_ITEM('')
SURFACE()
);
#31=(
BOUNDED_SURFACE()
B_SPLINE_SURFACE(5,1,((#28637,#28638),(#28639,#28640),(#28641,#28642),(#28643,
#28644),(#28645,#28646),(#28647,#28648),(#28649,#28650),(#28651,#28652),
(#28653,#28654),(#28655,#28656),(#28657,#28658),(#28659,#28660),(#28661,
#28662),(#28663,#28664),(#28665,#28666),(#28667,#28668),(#28669,#28670),
(#28671,#28672),(#28673,#28674),(#28675,#28676),(#28677,#28678),(#28679,
#28680),(#28681,#28682),(#28683,#28684),(#28685,#28686),(#28687,#28688),
(#28689,#28690),(#28691,#28692),(#28693,#28694),(#28695,#28696),(#28697,
#28698),(#28699,#28700),(#28701,#28702),(#28703,#28704),(#28705,#28706),
(#28707,#28708),(#28709,#28710),(#28711,#28712),(#28713,#28714),(#28715,
#28716),(#28717,#28718),(#28719,#28720),(#28721,#28722),(#28723,#28724),
(#28725,#28726),(#28727,#28728),(#28729,#28730),(#28731,#28732),(#28733,
#28734),(#28735,#28736),(#28737,#28738),(#28739,#28740),(#28741,#28742),
(#28743,#28744),(#28745,#28746),(#28747,#28748),(#28749,#28750),(#28751,
#28752),(#28753,#28754),(#28755,#28756),(#28757,#28758),(#28759,#28760),
(#28761,#28762),(#28763,#28764),(#28765,#28766),(#28767,#28768),(#28769,
#28770),(#28771,#28772),(#28773,#28774),(#28775,#28776)),.UNSPECIFIED.,
 .F.,.F.,.F.)
B_SPLINE_SURFACE_WITH_KNOTS((6,1,1,1,1,1,1,1,1,1,1,1,1,1,1,1,1,1,1,1,1,
1,1,1,1,1,1,1,1,1,1,1,1,1,1,1,1,1,1,1,1,1,1,1,1,1,1,1,1,1,1,1,1,1,1,1,1,
1,1,1,1,1,1,1,1,6),(2,2),(-1.,-0.984615384615383,-0.969230769230768,-0.953846153846152,
-0.938461538461537,-0.923076923076922,-0.907692307692306,-0.892307692307691,
-0.876923076923076,-0.86153846153846,-0.846153846153845,-0.83076923076923,
-0.815384615384614,-0.799999999999999,-0.784615384615384,-0.769230769230768,
-0.753846153846153,-0.738461538461538,-0.723076923076922,-0.707692307692307,
-0.692307692307692,-0.676923076923076,-0.661538461538461,-0.646153846153846,
-0.63076923076923,-0.615384615384615,-0.6,-0.584615384615384,-0.569230769230769,
-0.553846153846154,-0.538461538461538,-0.523076923076923,-0.507692307692308,
-0.492307692307692,-0.476923076923077,-0.461538461538462,-0.446153846153846,
-0.430769230769231,-0.415384615384615,-0.4,-0.384615384615385,-0.369230769230769,
-0.353846153846154,-0.338461538461538,-0.323076923076923,-0.307692307692308,
-0.292307692307692,-0.276923076923077,-0.261538461538462,-0.246153846153846,
-0.230769230769231,-0.215384615384615,-0.2,-0.184615384615385,-0.169230769230769,
-0.153846153846154,-0.138461538461538,-0.123076923076923,-0.107692307692308,
-0.0923076923076923,-0.0769230769230769,-0.0615384615384615,-0.0461538461538462,
-0.0307692307692308,-0.0153846153846154,0.),(-1.,1.),.UNSPECIFIED.)
GEOMETRIC_REPRESENTATION_ITEM()
RATIONAL_B_SPLINE_SURFACE(((1.,1.),(1.,1.),(1.,1.),(1.,1.),(1.,1.),(1.,
1.),(1.,1.),(1.,1.),(1.,1.),(1.,1.),(1.,1.),(1.,1.),(1.,1.),(1.,1.),(1.,
1.),(1.,1.),(1.,1.),(1.,1.),(1.,1.),(1.,1.),(1.,1.),(1.,1.),(1.,1.),(1.,
1.),(1.,1.),(1.,1.),(1.,1.),(1.,1.),(1.,1.),(1.,1.),(1.,1.),(1.,1.),(1.,
1.),(1.,1.),(1.,1.),(1.,1.),(1.,1.),(1.,1.),(1.,1.),(1.,1.),(1.,1.),(1.,
1.),(1.,1.),(1.,1.),(1.,1.),(1.,1.),(1.,1.),(1.,1.),(1.,1.),(1.,1.),(1.,
1.),(1.,1.),(1.,1.),(1.,1.),(1.,1.),(1.,1.),(1.,1.),(1.,1.),(1.,1.),(1.,
1.),(1.,1.),(1.,1.),(1.,1.),(1.,1.),(1.,1.),(1.,1.),(1.,1.),(1.,1.),(1.,
1.),(1.,1.)))
REPRESENTATION_ITEM('')
SURFACE()
);
#32=(
BOUNDED_SURFACE()
B_SPLINE_SURFACE(5,1,((#28853,#28854),(#28855,#28856),(#28857,#28858),(#28859,
#28860),(#28861,#28862),(#28863,#28864),(#28865,#28866),(#28867,#28868),
(#28869,#28870),(#28871,#28872),(#28873,#28874),(#28875,#28876),(#28877,
#28878),(#28879,#28880),(#28881,#28882),(#28883,#28884),(#28885,#28886),
(#28887,#28888),(#28889,#28890),(#28891,#28892),(#28893,#28894),(#28895,
#28896),(#28897,#28898),(#28899,#28900),(#28901,#28902),(#28903,#28904),
(#28905,#28906),(#28907,#28908),(#28909,#28910),(#28911,#28912),(#28913,
#28914),(#28915,#28916),(#28917,#28918),(#28919,#28920),(#28921,#28922),
(#28923,#28924),(#28925,#28926),(#28927,#28928),(#28929,#28930),(#28931,
#28932),(#28933,#28934),(#28935,#28936),(#28937,#28938),(#28939,#28940),
(#28941,#28942),(#28943,#28944),(#28945,#28946),(#28947,#28948),(#28949,
#28950),(#28951,#28952),(#28953,#28954),(#28955,#28956),(#28957,#28958),
(#28959,#28960),(#28961,#28962),(#28963,#28964),(#28965,#28966),(#28967,
#28968),(#28969,#28970),(#28971,#28972),(#28973,#28974),(#28975,#28976),
(#28977,#28978),(#28979,#28980),(#28981,#28982),(#28983,#28984),(#28985,
#28986),(#28987,#28988),(#28989,#28990),(#28991,#28992)),.UNSPECIFIED.,
 .F.,.F.,.F.)
B_SPLINE_SURFACE_WITH_KNOTS((6,1,1,1,1,1,1,1,1,1,1,1,1,1,1,1,1,1,1,1,1,
1,1,1,1,1,1,1,1,1,1,1,1,1,1,1,1,1,1,1,1,1,1,1,1,1,1,1,1,1,1,1,1,1,1,1,1,
1,1,1,1,1,1,1,1,6),(2,2),(-1.,-0.984615384615383,-0.969230769230768,-0.953846153846152,
-0.938461538461537,-0.923076923076922,-0.907692307692306,-0.892307692307691,
-0.876923076923076,-0.86153846153846,-0.846153846153845,-0.83076923076923,
-0.815384615384614,-0.799999999999999,-0.784615384615384,-0.769230769230768,
-0.753846153846153,-0.738461538461538,-0.723076923076922,-0.707692307692307,
-0.692307692307692,-0.676923076923076,-0.661538461538461,-0.646153846153846,
-0.63076923076923,-0.615384615384615,-0.6,-0.584615384615384,-0.569230769230769,
-0.553846153846154,-0.538461538461538,-0.523076923076923,-0.507692307692308,
-0.492307692307692,-0.476923076923077,-0.461538461538462,-0.446153846153846,
-0.430769230769231,-0.415384615384615,-0.4,-0.384615384615385,-0.369230769230769,
-0.353846153846154,-0.338461538461538,-0.323076923076923,-0.307692307692308,
-0.292307692307692,-0.276923076923077,-0.261538461538462,-0.246153846153846,
-0.230769230769231,-0.215384615384615,-0.2,-0.184615384615385,-0.169230769230769,
-0.153846153846154,-0.138461538461538,-0.123076923076923,-0.107692307692308,
-0.0923076923076923,-0.0769230769230769,-0.0615384615384615,-0.0461538461538462,
-0.0307692307692308,-0.0153846153846154,0.),(-1.,1.),.UNSPECIFIED.)
GEOMETRIC_REPRESENTATION_ITEM()
RATIONAL_B_SPLINE_SURFACE(((1.,1.),(1.,1.),(1.,1.),(1.,1.),(1.,1.),(1.,
1.),(1.,1.),(1.,1.),(1.,1.),(1.,1.),(1.,1.),(1.,1.),(1.,1.),(1.,1.),(1.,
1.),(1.,1.),(1.,1.),(1.,1.),(1.,1.),(1.,1.),(1.,1.),(1.,1.),(1.,1.),(1.,
1.),(1.,1.),(1.,1.),(1.,1.),(1.,1.),(1.,1.),(1.,1.),(1.,1.),(1.,1.),(1.,
1.),(1.,1.),(1.,1.),(1.,1.),(1.,1.),(1.,1.),(1.,1.),(1.,1.),(1.,1.),(1.,
1.),(1.,1.),(1.,1.),(1.,1.),(1.,1.),(1.,1.),(1.,1.),(1.,1.),(1.,1.),(1.,
1.),(1.,1.),(1.,1.),(1.,1.),(1.,1.),(1.,1.),(1.,1.),(1.,1.),(1.,1.),(1.,
1.),(1.,1.),(1.,1.),(1.,1.),(1.,1.),(1.,1.),(1.,1.),(1.,1.),(1.,1.),(1.,
1.),(1.,1.)))
REPRESENTATION_ITEM('')
SURFACE()
);
#33=(
BOUNDED_SURFACE()
B_SPLINE_SURFACE(5,1,((#29069,#29070),(#29071,#29072),(#29073,#29074),(#29075,
#29076),(#29077,#29078),(#29079,#29080),(#29081,#29082),(#29083,#29084),
(#29085,#29086),(#29087,#29088),(#29089,#29090),(#29091,#29092),(#29093,
#29094),(#29095,#29096),(#29097,#29098),(#29099,#29100),(#29101,#29102),
(#29103,#29104),(#29105,#29106),(#29107,#29108),(#29109,#29110),(#29111,
#29112),(#29113,#29114),(#29115,#29116),(#29117,#29118),(#29119,#29120),
(#29121,#29122),(#29123,#29124),(#29125,#29126),(#29127,#29128),(#29129,
#29130),(#29131,#29132),(#29133,#29134),(#29135,#29136),(#29137,#29138),
(#29139,#29140),(#29141,#29142),(#29143,#29144),(#29145,#29146),(#29147,
#29148),(#29149,#29150),(#29151,#29152),(#29153,#29154),(#29155,#29156),
(#29157,#29158),(#29159,#29160),(#29161,#29162),(#29163,#29164),(#29165,
#29166),(#29167,#29168),(#29169,#29170),(#29171,#29172),(#29173,#29174),
(#29175,#29176),(#29177,#29178),(#29179,#29180),(#29181,#29182),(#29183,
#29184),(#29185,#29186),(#29187,#29188),(#29189,#29190),(#29191,#29192),
(#29193,#29194),(#29195,#29196),(#29197,#29198),(#29199,#29200),(#29201,
#29202),(#29203,#29204),(#29205,#29206),(#29207,#29208)),.UNSPECIFIED.,
 .F.,.F.,.F.)
B_SPLINE_SURFACE_WITH_KNOTS((6,1,1,1,1,1,1,1,1,1,1,1,1,1,1,1,1,1,1,1,1,
1,1,1,1,1,1,1,1,1,1,1,1,1,1,1,1,1,1,1,1,1,1,1,1,1,1,1,1,1,1,1,1,1,1,1,1,
1,1,1,1,1,1,1,1,6),(2,2),(-1.,-0.984615384615383,-0.969230769230768,-0.953846153846152,
-0.938461538461537,-0.923076923076922,-0.907692307692306,-0.892307692307691,
-0.876923076923076,-0.86153846153846,-0.846153846153845,-0.83076923076923,
-0.815384615384614,-0.799999999999999,-0.784615384615384,-0.769230769230768,
-0.753846153846153,-0.738461538461538,-0.723076923076922,-0.707692307692307,
-0.692307692307692,-0.676923076923076,-0.661538461538461,-0.646153846153846,
-0.63076923076923,-0.615384615384615,-0.6,-0.584615384615384,-0.569230769230769,
-0.553846153846154,-0.538461538461538,-0.523076923076923,-0.507692307692308,
-0.492307692307692,-0.476923076923077,-0.461538461538462,-0.446153846153846,
-0.430769230769231,-0.415384615384615,-0.4,-0.384615384615385,-0.369230769230769,
-0.353846153846154,-0.338461538461538,-0.323076923076923,-0.307692307692308,
-0.292307692307692,-0.276923076923077,-0.261538461538462,-0.246153846153846,
-0.230769230769231,-0.215384615384615,-0.2,-0.184615384615385,-0.169230769230769,
-0.153846153846154,-0.138461538461538,-0.123076923076923,-0.107692307692308,
-0.0923076923076923,-0.0769230769230769,-0.0615384615384615,-0.0461538461538462,
-0.0307692307692308,-0.0153846153846154,0.),(-1.,1.),.UNSPECIFIED.)
GEOMETRIC_REPRESENTATION_ITEM()
RATIONAL_B_SPLINE_SURFACE(((1.,1.),(1.,1.),(1.,1.),(1.,1.),(1.,1.),(1.,
1.),(1.,1.),(1.,1.),(1.,1.),(1.,1.),(1.,1.),(1.,1.),(1.,1.),(1.,1.),(1.,
1.),(1.,1.),(1.,1.),(1.,1.),(1.,1.),(1.,1.),(1.,1.),(1.,1.),(1.,1.),(1.,
1.),(1.,1.),(1.,1.),(1.,1.),(1.,1.),(1.,1.),(1.,1.),(1.,1.),(1.,1.),(1.,
1.),(1.,1.),(1.,1.),(1.,1.),(1.,1.),(1.,1.),(1.,1.),(1.,1.),(1.,1.),(1.,
1.),(1.,1.),(1.,1.),(1.,1.),(1.,1.),(1.,1.),(1.,1.),(1.,1.),(1.,1.),(1.,
1.),(1.,1.),(1.,1.),(1.,1.),(1.,1.),(1.,1.),(1.,1.),(1.,1.),(1.,1.),(1.,
1.),(1.,1.),(1.,1.),(1.,1.),(1.,1.),(1.,1.),(1.,1.),(1.,1.),(1.,1.),(1.,
1.),(1.,1.)))
REPRESENTATION_ITEM('')
SURFACE()
);
#34=(
BOUNDED_SURFACE()
B_SPLINE_SURFACE(5,1,((#29285,#29286),(#29287,#29288),(#29289,#29290),(#29291,
#29292),(#29293,#29294),(#29295,#29296),(#29297,#29298),(#29299,#29300),
(#29301,#29302),(#29303,#29304),(#29305,#29306),(#29307,#29308),(#29309,
#29310),(#29311,#29312),(#29313,#29314),(#29315,#29316),(#29317,#29318),
(#29319,#29320),(#29321,#29322),(#29323,#29324),(#29325,#29326),(#29327,
#29328),(#29329,#29330),(#29331,#29332),(#29333,#29334),(#29335,#29336),
(#29337,#29338),(#29339,#29340),(#29341,#29342),(#29343,#29344),(#29345,
#29346),(#29347,#29348),(#29349,#29350),(#29351,#29352),(#29353,#29354),
(#29355,#29356),(#29357,#29358),(#29359,#29360),(#29361,#29362),(#29363,
#29364),(#29365,#29366),(#29367,#29368),(#29369,#29370),(#29371,#29372),
(#29373,#29374),(#29375,#29376),(#29377,#29378),(#29379,#29380),(#29381,
#29382),(#29383,#29384),(#29385,#29386),(#29387,#29388),(#29389,#29390),
(#29391,#29392),(#29393,#29394),(#29395,#29396),(#29397,#29398),(#29399,
#29400),(#29401,#29402),(#29403,#29404),(#29405,#29406),(#29407,#29408),
(#29409,#29410),(#29411,#29412),(#29413,#29414),(#29415,#29416),(#29417,
#29418),(#29419,#29420),(#29421,#29422),(#29423,#29424)),.UNSPECIFIED.,
 .F.,.F.,.F.)
B_SPLINE_SURFACE_WITH_KNOTS((6,1,1,1,1,1,1,1,1,1,1,1,1,1,1,1,1,1,1,1,1,
1,1,1,1,1,1,1,1,1,1,1,1,1,1,1,1,1,1,1,1,1,1,1,1,1,1,1,1,1,1,1,1,1,1,1,1,
1,1,1,1,1,1,1,1,6),(2,2),(-1.,-0.984615384615383,-0.969230769230768,-0.953846153846152,
-0.938461538461537,-0.923076923076922,-0.907692307692306,-0.892307692307691,
-0.876923076923076,-0.86153846153846,-0.846153846153845,-0.83076923076923,
-0.815384615384614,-0.799999999999999,-0.784615384615384,-0.769230769230768,
-0.753846153846153,-0.738461538461538,-0.723076923076922,-0.707692307692307,
-0.692307692307692,-0.676923076923076,-0.661538461538461,-0.646153846153846,
-0.63076923076923,-0.615384615384615,-0.6,-0.584615384615384,-0.569230769230769,
-0.553846153846154,-0.538461538461538,-0.523076923076923,-0.507692307692308,
-0.492307692307692,-0.476923076923077,-0.461538461538462,-0.446153846153846,
-0.430769230769231,-0.415384615384615,-0.4,-0.384615384615385,-0.369230769230769,
-0.353846153846154,-0.338461538461538,-0.323076923076923,-0.307692307692308,
-0.292307692307692,-0.276923076923077,-0.261538461538462,-0.246153846153846,
-0.230769230769231,-0.215384615384615,-0.2,-0.184615384615385,-0.169230769230769,
-0.153846153846154,-0.138461538461538,-0.123076923076923,-0.107692307692308,
-0.0923076923076923,-0.0769230769230769,-0.0615384615384615,-0.0461538461538462,
-0.0307692307692308,-0.0153846153846154,0.),(-1.,1.),.UNSPECIFIED.)
GEOMETRIC_REPRESENTATION_ITEM()
RATIONAL_B_SPLINE_SURFACE(((1.,1.),(1.,1.),(1.,1.),(1.,1.),(1.,1.),(1.,
1.),(1.,1.),(1.,1.),(1.,1.),(1.,1.),(1.,1.),(1.,1.),(1.,1.),(1.,1.),(1.,
1.),(1.,1.),(1.,1.),(1.,1.),(1.,1.),(1.,1.),(1.,1.),(1.,1.),(1.,1.),(1.,
1.),(1.,1.),(1.,1.),(1.,1.),(1.,1.),(1.,1.),(1.,1.),(1.,1.),(1.,1.),(1.,
1.),(1.,1.),(1.,1.),(1.,1.),(1.,1.),(1.,1.),(1.,1.),(1.,1.),(1.,1.),(1.,
1.),(1.,1.),(1.,1.),(1.,1.),(1.,1.),(1.,1.),(1.,1.),(1.,1.),(1.,1.),(1.,
1.),(1.,1.),(1.,1.),(1.,1.),(1.,1.),(1.,1.),(1.,1.),(1.,1.),(1.,1.),(1.,
1.),(1.,1.),(1.,1.),(1.,1.),(1.,1.),(1.,1.),(1.,1.),(1.,1.),(1.,1.),(1.,
1.),(1.,1.)))
REPRESENTATION_ITEM('')
SURFACE()
);
#35=(
BOUNDED_SURFACE()
B_SPLINE_SURFACE(5,1,((#29501,#29502),(#29503,#29504),(#29505,#29506),(#29507,
#29508),(#29509,#29510),(#29511,#29512),(#29513,#29514),(#29515,#29516),
(#29517,#29518),(#29519,#29520),(#29521,#29522),(#29523,#29524),(#29525,
#29526),(#29527,#29528),(#29529,#29530),(#29531,#29532),(#29533,#29534),
(#29535,#29536),(#29537,#29538),(#29539,#29540),(#29541,#29542),(#29543,
#29544),(#29545,#29546),(#29547,#29548),(#29549,#29550),(#29551,#29552),
(#29553,#29554),(#29555,#29556),(#29557,#29558),(#29559,#29560),(#29561,
#29562),(#29563,#29564),(#29565,#29566),(#29567,#29568),(#29569,#29570),
(#29571,#29572),(#29573,#29574),(#29575,#29576),(#29577,#29578),(#29579,
#29580),(#29581,#29582),(#29583,#29584),(#29585,#29586),(#29587,#29588),
(#29589,#29590),(#29591,#29592),(#29593,#29594),(#29595,#29596),(#29597,
#29598),(#29599,#29600),(#29601,#29602),(#29603,#29604),(#29605,#29606),
(#29607,#29608),(#29609,#29610),(#29611,#29612),(#29613,#29614),(#29615,
#29616),(#29617,#29618),(#29619,#29620),(#29621,#29622),(#29623,#29624),
(#29625,#29626),(#29627,#29628),(#29629,#29630),(#29631,#29632),(#29633,
#29634),(#29635,#29636),(#29637,#29638),(#29639,#29640)),.UNSPECIFIED.,
 .F.,.F.,.F.)
B_SPLINE_SURFACE_WITH_KNOTS((6,1,1,1,1,1,1,1,1,1,1,1,1,1,1,1,1,1,1,1,1,
1,1,1,1,1,1,1,1,1,1,1,1,1,1,1,1,1,1,1,1,1,1,1,1,1,1,1,1,1,1,1,1,1,1,1,1,
1,1,1,1,1,1,1,1,6),(2,2),(-1.,-0.984615384615383,-0.969230769230768,-0.953846153846152,
-0.938461538461537,-0.923076923076922,-0.907692307692306,-0.892307692307691,
-0.876923076923076,-0.86153846153846,-0.846153846153845,-0.83076923076923,
-0.815384615384614,-0.799999999999999,-0.784615384615384,-0.769230769230768,
-0.753846153846153,-0.738461538461538,-0.723076923076922,-0.707692307692307,
-0.692307692307692,-0.676923076923076,-0.661538461538461,-0.646153846153846,
-0.63076923076923,-0.615384615384615,-0.6,-0.584615384615384,-0.569230769230769,
-0.553846153846154,-0.538461538461538,-0.523076923076923,-0.507692307692308,
-0.492307692307692,-0.476923076923077,-0.461538461538462,-0.446153846153846,
-0.430769230769231,-0.415384615384615,-0.4,-0.384615384615385,-0.369230769230769,
-0.353846153846154,-0.338461538461538,-0.323076923076923,-0.307692307692308,
-0.292307692307692,-0.276923076923077,-0.261538461538462,-0.246153846153846,
-0.230769230769231,-0.215384615384615,-0.2,-0.184615384615385,-0.169230769230769,
-0.153846153846154,-0.138461538461538,-0.123076923076923,-0.107692307692308,
-0.0923076923076923,-0.0769230769230769,-0.0615384615384615,-0.0461538461538462,
-0.0307692307692308,-0.0153846153846154,0.),(-1.,1.),.UNSPECIFIED.)
GEOMETRIC_REPRESENTATION_ITEM()
RATIONAL_B_SPLINE_SURFACE(((1.,1.),(1.,1.),(1.,1.),(1.,1.),(1.,1.),(1.,
1.),(1.,1.),(1.,1.),(1.,1.),(1.,1.),(1.,1.),(1.,1.),(1.,1.),(1.,1.),(1.,
1.),(1.,1.),(1.,1.),(1.,1.),(1.,1.),(1.,1.),(1.,1.),(1.,1.),(1.,1.),(1.,
1.),(1.,1.),(1.,1.),(1.,1.),(1.,1.),(1.,1.),(1.,1.),(1.,1.),(1.,1.),(1.,
1.),(1.,1.),(1.,1.),(1.,1.),(1.,1.),(1.,1.),(1.,1.),(1.,1.),(1.,1.),(1.,
1.),(1.,1.),(1.,1.),(1.,1.),(1.,1.),(1.,1.),(1.,1.),(1.,1.),(1.,1.),(1.,
1.),(1.,1.),(1.,1.),(1.,1.),(1.,1.),(1.,1.),(1.,1.),(1.,1.),(1.,1.),(1.,
1.),(1.,1.),(1.,1.),(1.,1.),(1.,1.),(1.,1.),(1.,1.),(1.,1.),(1.,1.),(1.,
1.),(1.,1.)))
REPRESENTATION_ITEM('')
SURFACE()
);
#36=(
BOUNDED_SURFACE()
B_SPLINE_SURFACE(5,1,((#29717,#29718),(#29719,#29720),(#29721,#29722),(#29723,
#29724),(#29725,#29726),(#29727,#29728),(#29729,#29730),(#29731,#29732),
(#29733,#29734),(#29735,#29736),(#29737,#29738),(#29739,#29740),(#29741,
#29742),(#29743,#29744),(#29745,#29746),(#29747,#29748),(#29749,#29750),
(#29751,#29752),(#29753,#29754),(#29755,#29756),(#29757,#29758),(#29759,
#29760),(#29761,#29762),(#29763,#29764),(#29765,#29766),(#29767,#29768),
(#29769,#29770),(#29771,#29772),(#29773,#29774),(#29775,#29776),(#29777,
#29778),(#29779,#29780),(#29781,#29782),(#29783,#29784),(#29785,#29786),
(#29787,#29788),(#29789,#29790),(#29791,#29792),(#29793,#29794),(#29795,
#29796),(#29797,#29798),(#29799,#29800),(#29801,#29802),(#29803,#29804),
(#29805,#29806),(#29807,#29808),(#29809,#29810),(#29811,#29812),(#29813,
#29814),(#29815,#29816),(#29817,#29818),(#29819,#29820),(#29821,#29822),
(#29823,#29824),(#29825,#29826),(#29827,#29828),(#29829,#29830),(#29831,
#29832),(#29833,#29834),(#29835,#29836),(#29837,#29838),(#29839,#29840),
(#29841,#29842),(#29843,#29844),(#29845,#29846),(#29847,#29848),(#29849,
#29850),(#29851,#29852),(#29853,#29854),(#29855,#29856)),.UNSPECIFIED.,
 .F.,.F.,.F.)
B_SPLINE_SURFACE_WITH_KNOTS((6,1,1,1,1,1,1,1,1,1,1,1,1,1,1,1,1,1,1,1,1,
1,1,1,1,1,1,1,1,1,1,1,1,1,1,1,1,1,1,1,1,1,1,1,1,1,1,1,1,1,1,1,1,1,1,1,1,
1,1,1,1,1,1,1,1,6),(2,2),(-1.,-0.984615384615383,-0.969230769230768,-0.953846153846152,
-0.938461538461537,-0.923076923076922,-0.907692307692306,-0.892307692307691,
-0.876923076923076,-0.86153846153846,-0.846153846153845,-0.83076923076923,
-0.815384615384614,-0.799999999999999,-0.784615384615384,-0.769230769230768,
-0.753846153846153,-0.738461538461538,-0.723076923076922,-0.707692307692307,
-0.692307692307692,-0.676923076923076,-0.661538461538461,-0.646153846153846,
-0.63076923076923,-0.615384615384615,-0.6,-0.584615384615384,-0.569230769230769,
-0.553846153846154,-0.538461538461538,-0.523076923076923,-0.507692307692308,
-0.492307692307692,-0.476923076923077,-0.461538461538462,-0.446153846153846,
-0.430769230769231,-0.415384615384615,-0.4,-0.384615384615385,-0.369230769230769,
-0.353846153846154,-0.338461538461538,-0.323076923076923,-0.307692307692308,
-0.292307692307692,-0.276923076923077,-0.261538461538462,-0.246153846153846,
-0.230769230769231,-0.215384615384615,-0.2,-0.184615384615385,-0.169230769230769,
-0.153846153846154,-0.138461538461538,-0.123076923076923,-0.107692307692308,
-0.0923076923076923,-0.0769230769230769,-0.0615384615384615,-0.0461538461538462,
-0.0307692307692308,-0.0153846153846154,0.),(-1.,1.),.UNSPECIFIED.)
GEOMETRIC_REPRESENTATION_ITEM()
RATIONAL_B_SPLINE_SURFACE(((1.,1.),(1.,1.),(1.,1.),(1.,1.),(1.,1.),(1.,
1.),(1.,1.),(1.,1.),(1.,1.),(1.,1.),(1.,1.),(1.,1.),(1.,1.),(1.,1.),(1.,
1.),(1.,1.),(1.,1.),(1.,1.),(1.,1.),(1.,1.),(1.,1.),(1.,1.),(1.,1.),(1.,
1.),(1.,1.),(1.,1.),(1.,1.),(1.,1.),(1.,1.),(1.,1.),(1.,1.),(1.,1.),(1.,
1.),(1.,1.),(1.,1.),(1.,1.),(1.,1.),(1.,1.),(1.,1.),(1.,1.),(1.,1.),(1.,
1.),(1.,1.),(1.,1.),(1.,1.),(1.,1.),(1.,1.),(1.,1.),(1.,1.),(1.,1.),(1.,
1.),(1.,1.),(1.,1.),(1.,1.),(1.,1.),(1.,1.),(1.,1.),(1.,1.),(1.,1.),(1.,
1.),(1.,1.),(1.,1.),(1.,1.),(1.,1.),(1.,1.),(1.,1.),(1.,1.),(1.,1.),(1.,
1.),(1.,1.)))
REPRESENTATION_ITEM('')
SURFACE()
);
#37=(
BOUNDED_SURFACE()
B_SPLINE_SURFACE(5,1,((#29933,#29934),(#29935,#29936),(#29937,#29938),(#29939,
#29940),(#29941,#29942),(#29943,#29944),(#29945,#29946),(#29947,#29948),
(#29949,#29950),(#29951,#29952),(#29953,#29954),(#29955,#29956),(#29957,
#29958),(#29959,#29960),(#29961,#29962),(#29963,#29964),(#29965,#29966),
(#29967,#29968),(#29969,#29970),(#29971,#29972),(#29973,#29974),(#29975,
#29976),(#29977,#29978),(#29979,#29980),(#29981,#29982),(#29983,#29984),
(#29985,#29986),(#29987,#29988),(#29989,#29990),(#29991,#29992),(#29993,
#29994),(#29995,#29996),(#29997,#29998),(#29999,#30000),(#30001,#30002),
(#30003,#30004),(#30005,#30006),(#30007,#30008),(#30009,#30010),(#30011,
#30012),(#30013,#30014),(#30015,#30016),(#30017,#30018),(#30019,#30020),
(#30021,#30022),(#30023,#30024),(#30025,#30026),(#30027,#30028),(#30029,
#30030),(#30031,#30032),(#30033,#30034),(#30035,#30036),(#30037,#30038),
(#30039,#30040),(#30041,#30042),(#30043,#30044),(#30045,#30046),(#30047,
#30048),(#30049,#30050),(#30051,#30052),(#30053,#30054),(#30055,#30056),
(#30057,#30058),(#30059,#30060),(#30061,#30062),(#30063,#30064),(#30065,
#30066),(#30067,#30068),(#30069,#30070),(#30071,#30072)),.UNSPECIFIED.,
 .F.,.F.,.F.)
B_SPLINE_SURFACE_WITH_KNOTS((6,1,1,1,1,1,1,1,1,1,1,1,1,1,1,1,1,1,1,1,1,
1,1,1,1,1,1,1,1,1,1,1,1,1,1,1,1,1,1,1,1,1,1,1,1,1,1,1,1,1,1,1,1,1,1,1,1,
1,1,1,1,1,1,1,1,6),(2,2),(-1.,-0.984615384615383,-0.969230769230768,-0.953846153846152,
-0.938461538461537,-0.923076923076922,-0.907692307692306,-0.892307692307691,
-0.876923076923076,-0.86153846153846,-0.846153846153845,-0.83076923076923,
-0.815384615384614,-0.799999999999999,-0.784615384615384,-0.769230769230768,
-0.753846153846153,-0.738461538461538,-0.723076923076922,-0.707692307692307,
-0.692307692307692,-0.676923076923076,-0.661538461538461,-0.646153846153846,
-0.63076923076923,-0.615384615384615,-0.6,-0.584615384615384,-0.569230769230769,
-0.553846153846154,-0.538461538461538,-0.523076923076923,-0.507692307692308,
-0.492307692307692,-0.476923076923077,-0.461538461538462,-0.446153846153846,
-0.430769230769231,-0.415384615384615,-0.4,-0.384615384615385,-0.369230769230769,
-0.353846153846154,-0.338461538461538,-0.323076923076923,-0.307692307692308,
-0.292307692307692,-0.276923076923077,-0.261538461538462,-0.246153846153846,
-0.230769230769231,-0.215384615384615,-0.2,-0.184615384615385,-0.169230769230769,
-0.153846153846154,-0.138461538461538,-0.123076923076923,-0.107692307692308,
-0.0923076923076923,-0.0769230769230769,-0.0615384615384615,-0.0461538461538462,
-0.0307692307692308,-0.0153846153846154,0.),(-1.,1.),.UNSPECIFIED.)
GEOMETRIC_REPRESENTATION_ITEM()
RATIONAL_B_SPLINE_SURFACE(((1.,1.),(1.,1.),(1.,1.),(1.,1.),(1.,1.),(1.,
1.),(1.,1.),(1.,1.),(1.,1.),(1.,1.),(1.,1.),(1.,1.),(1.,1.),(1.,1.),(1.,
1.),(1.,1.),(1.,1.),(1.,1.),(1.,1.),(1.,1.),(1.,1.),(1.,1.),(1.,1.),(1.,
1.),(1.,1.),(1.,1.),(1.,1.),(1.,1.),(1.,1.),(1.,1.),(1.,1.),(1.,1.),(1.,
1.),(1.,1.),(1.,1.),(1.,1.),(1.,1.),(1.,1.),(1.,1.),(1.,1.),(1.,1.),(1.,
1.),(1.,1.),(1.,1.),(1.,1.),(1.,1.),(1.,1.),(1.,1.),(1.,1.),(1.,1.),(1.,
1.),(1.,1.),(1.,1.),(1.,1.),(1.,1.),(1.,1.),(1.,1.),(1.,1.),(1.,1.),(1.,
1.),(1.,1.),(1.,1.),(1.,1.),(1.,1.),(1.,1.),(1.,1.),(1.,1.),(1.,1.),(1.,
1.),(1.,1.)))
REPRESENTATION_ITEM('')
SURFACE()
);
#38=(
BOUNDED_SURFACE()
B_SPLINE_SURFACE(5,1,((#30149,#30150),(#30151,#30152),(#30153,#30154),(#30155,
#30156),(#30157,#30158),(#30159,#30160),(#30161,#30162),(#30163,#30164),
(#30165,#30166),(#30167,#30168),(#30169,#30170),(#30171,#30172),(#30173,
#30174),(#30175,#30176),(#30177,#30178),(#30179,#30180),(#30181,#30182),
(#30183,#30184),(#30185,#30186),(#30187,#30188),(#30189,#30190),(#30191,
#30192),(#30193,#30194),(#30195,#30196),(#30197,#30198),(#30199,#30200),
(#30201,#30202),(#30203,#30204),(#30205,#30206),(#30207,#30208),(#30209,
#30210),(#30211,#30212),(#30213,#30214),(#30215,#30216),(#30217,#30218),
(#30219,#30220),(#30221,#30222),(#30223,#30224),(#30225,#30226),(#30227,
#30228),(#30229,#30230),(#30231,#30232),(#30233,#30234),(#30235,#30236),
(#30237,#30238),(#30239,#30240),(#30241,#30242),(#30243,#30244),(#30245,
#30246),(#30247,#30248),(#30249,#30250),(#30251,#30252),(#30253,#30254),
(#30255,#30256),(#30257,#30258),(#30259,#30260),(#30261,#30262),(#30263,
#30264),(#30265,#30266),(#30267,#30268),(#30269,#30270),(#30271,#30272),
(#30273,#30274),(#30275,#30276),(#30277,#30278),(#30279,#30280),(#30281,
#30282),(#30283,#30284),(#30285,#30286),(#30287,#30288)),.UNSPECIFIED.,
 .F.,.F.,.F.)
B_SPLINE_SURFACE_WITH_KNOTS((6,1,1,1,1,1,1,1,1,1,1,1,1,1,1,1,1,1,1,1,1,
1,1,1,1,1,1,1,1,1,1,1,1,1,1,1,1,1,1,1,1,1,1,1,1,1,1,1,1,1,1,1,1,1,1,1,1,
1,1,1,1,1,1,1,1,6),(2,2),(-1.,-0.984615384615383,-0.969230769230768,-0.953846153846152,
-0.938461538461537,-0.923076923076922,-0.907692307692306,-0.892307692307691,
-0.876923076923076,-0.86153846153846,-0.846153846153845,-0.83076923076923,
-0.815384615384614,-0.799999999999999,-0.784615384615384,-0.769230769230768,
-0.753846153846153,-0.738461538461538,-0.723076923076922,-0.707692307692307,
-0.692307692307692,-0.676923076923076,-0.661538461538461,-0.646153846153846,
-0.63076923076923,-0.615384615384615,-0.6,-0.584615384615384,-0.569230769230769,
-0.553846153846154,-0.538461538461538,-0.523076923076923,-0.507692307692308,
-0.492307692307692,-0.476923076923077,-0.461538461538462,-0.446153846153846,
-0.430769230769231,-0.415384615384615,-0.4,-0.384615384615385,-0.369230769230769,
-0.353846153846154,-0.338461538461538,-0.323076923076923,-0.307692307692308,
-0.292307692307692,-0.276923076923077,-0.261538461538462,-0.246153846153846,
-0.230769230769231,-0.215384615384615,-0.2,-0.184615384615385,-0.169230769230769,
-0.153846153846154,-0.138461538461538,-0.123076923076923,-0.107692307692308,
-0.0923076923076923,-0.0769230769230769,-0.0615384615384615,-0.0461538461538462,
-0.0307692307692308,-0.0153846153846154,0.),(-1.,1.),.UNSPECIFIED.)
GEOMETRIC_REPRESENTATION_ITEM()
RATIONAL_B_SPLINE_SURFACE(((1.,1.),(1.,1.),(1.,1.),(1.,1.),(1.,1.),(1.,
1.),(1.,1.),(1.,1.),(1.,1.),(1.,1.),(1.,1.),(1.,1.),(1.,1.),(1.,1.),(1.,
1.),(1.,1.),(1.,1.),(1.,1.),(1.,1.),(1.,1.),(1.,1.),(1.,1.),(1.,1.),(1.,
1.),(1.,1.),(1.,1.),(1.,1.),(1.,1.),(1.,1.),(1.,1.),(1.,1.),(1.,1.),(1.,
1.),(1.,1.),(1.,1.),(1.,1.),(1.,1.),(1.,1.),(1.,1.),(1.,1.),(1.,1.),(1.,
1.),(1.,1.),(1.,1.),(1.,1.),(1.,1.),(1.,1.),(1.,1.),(1.,1.),(1.,1.),(1.,
1.),(1.,1.),(1.,1.),(1.,1.),(1.,1.),(1.,1.),(1.,1.),(1.,1.),(1.,1.),(1.,
1.),(1.,1.),(1.,1.),(1.,1.),(1.,1.),(1.,1.),(1.,1.),(1.,1.),(1.,1.),(1.,
1.),(1.,1.)))
REPRESENTATION_ITEM('')
SURFACE()
);
#39=(
BOUNDED_SURFACE()
B_SPLINE_SURFACE(5,1,((#30365,#30366),(#30367,#30368),(#30369,#30370),(#30371,
#30372),(#30373,#30374),(#30375,#30376),(#30377,#30378),(#30379,#30380),
(#30381,#30382),(#30383,#30384),(#30385,#30386),(#30387,#30388),(#30389,
#30390),(#30391,#30392),(#30393,#30394),(#30395,#30396),(#30397,#30398),
(#30399,#30400),(#30401,#30402),(#30403,#30404),(#30405,#30406),(#30407,
#30408),(#30409,#30410),(#30411,#30412),(#30413,#30414),(#30415,#30416),
(#30417,#30418),(#30419,#30420),(#30421,#30422),(#30423,#30424),(#30425,
#30426),(#30427,#30428),(#30429,#30430),(#30431,#30432),(#30433,#30434),
(#30435,#30436),(#30437,#30438),(#30439,#30440),(#30441,#30442),(#30443,
#30444),(#30445,#30446),(#30447,#30448),(#30449,#30450),(#30451,#30452),
(#30453,#30454),(#30455,#30456),(#30457,#30458),(#30459,#30460),(#30461,
#30462),(#30463,#30464),(#30465,#30466),(#30467,#30468),(#30469,#30470),
(#30471,#30472),(#30473,#30474),(#30475,#30476),(#30477,#30478),(#30479,
#30480),(#30481,#30482),(#30483,#30484),(#30485,#30486),(#30487,#30488),
(#30489,#30490),(#30491,#30492),(#30493,#30494),(#30495,#30496),(#30497,
#30498),(#30499,#30500),(#30501,#30502),(#30503,#30504)),.UNSPECIFIED.,
 .F.,.F.,.F.)
B_SPLINE_SURFACE_WITH_KNOTS((6,1,1,1,1,1,1,1,1,1,1,1,1,1,1,1,1,1,1,1,1,
1,1,1,1,1,1,1,1,1,1,1,1,1,1,1,1,1,1,1,1,1,1,1,1,1,1,1,1,1,1,1,1,1,1,1,1,
1,1,1,1,1,1,1,1,6),(2,2),(-1.,-0.984615384615383,-0.969230769230768,-0.953846153846152,
-0.938461538461537,-0.923076923076922,-0.907692307692306,-0.892307692307691,
-0.876923076923076,-0.86153846153846,-0.846153846153845,-0.83076923076923,
-0.815384615384614,-0.799999999999999,-0.784615384615384,-0.769230769230768,
-0.753846153846153,-0.738461538461538,-0.723076923076922,-0.707692307692307,
-0.692307692307692,-0.676923076923076,-0.661538461538461,-0.646153846153846,
-0.63076923076923,-0.615384615384615,-0.6,-0.584615384615384,-0.569230769230769,
-0.553846153846154,-0.538461538461538,-0.523076923076923,-0.507692307692308,
-0.492307692307692,-0.476923076923077,-0.461538461538462,-0.446153846153846,
-0.430769230769231,-0.415384615384615,-0.4,-0.384615384615385,-0.369230769230769,
-0.353846153846154,-0.338461538461538,-0.323076923076923,-0.307692307692308,
-0.292307692307692,-0.276923076923077,-0.261538461538462,-0.246153846153846,
-0.230769230769231,-0.215384615384615,-0.2,-0.184615384615385,-0.169230769230769,
-0.153846153846154,-0.138461538461538,-0.123076923076923,-0.107692307692308,
-0.0923076923076923,-0.0769230769230769,-0.0615384615384615,-0.0461538461538462,
-0.0307692307692308,-0.0153846153846154,0.),(-1.,1.),.UNSPECIFIED.)
GEOMETRIC_REPRESENTATION_ITEM()
RATIONAL_B_SPLINE_SURFACE(((1.,1.),(1.,1.),(1.,1.),(1.,1.),(1.,1.),(1.,
1.),(1.,1.),(1.,1.),(1.,1.),(1.,1.),(1.,1.),(1.,1.),(1.,1.),(1.,1.),(1.,
1.),(1.,1.),(1.,1.),(1.,1.),(1.,1.),(1.,1.),(1.,1.),(1.,1.),(1.,1.),(1.,
1.),(1.,1.),(1.,1.),(1.,1.),(1.,1.),(1.,1.),(1.,1.),(1.,1.),(1.,1.),(1.,
1.),(1.,1.),(1.,1.),(1.,1.),(1.,1.),(1.,1.),(1.,1.),(1.,1.),(1.,1.),(1.,
1.),(1.,1.),(1.,1.),(1.,1.),(1.,1.),(1.,1.),(1.,1.),(1.,1.),(1.,1.),(1.,
1.),(1.,1.),(1.,1.),(1.,1.),(1.,1.),(1.,1.),(1.,1.),(1.,1.),(1.,1.),(1.,
1.),(1.,1.),(1.,1.),(1.,1.),(1.,1.),(1.,1.),(1.,1.),(1.,1.),(1.,1.),(1.,
1.),(1.,1.)))
REPRESENTATION_ITEM('')
SURFACE()
);
#40=(
BOUNDED_SURFACE()
B_SPLINE_SURFACE(5,1,((#30581,#30582),(#30583,#30584),(#30585,#30586),(#30587,
#30588),(#30589,#30590),(#30591,#30592),(#30593,#30594),(#30595,#30596),
(#30597,#30598),(#30599,#30600),(#30601,#30602),(#30603,#30604),(#30605,
#30606),(#30607,#30608),(#30609,#30610),(#30611,#30612),(#30613,#30614),
(#30615,#30616),(#30617,#30618),(#30619,#30620),(#30621,#30622),(#30623,
#30624),(#30625,#30626),(#30627,#30628),(#30629,#30630),(#30631,#30632),
(#30633,#30634),(#30635,#30636),(#30637,#30638),(#30639,#30640),(#30641,
#30642),(#30643,#30644),(#30645,#30646),(#30647,#30648),(#30649,#30650),
(#30651,#30652),(#30653,#30654),(#30655,#30656),(#30657,#30658),(#30659,
#30660),(#30661,#30662),(#30663,#30664),(#30665,#30666),(#30667,#30668),
(#30669,#30670),(#30671,#30672),(#30673,#30674),(#30675,#30676),(#30677,
#30678),(#30679,#30680),(#30681,#30682),(#30683,#30684),(#30685,#30686),
(#30687,#30688),(#30689,#30690),(#30691,#30692),(#30693,#30694),(#30695,
#30696),(#30697,#30698),(#30699,#30700),(#30701,#30702),(#30703,#30704),
(#30705,#30706),(#30707,#30708),(#30709,#30710),(#30711,#30712),(#30713,
#30714),(#30715,#30716),(#30717,#30718),(#30719,#30720)),.UNSPECIFIED.,
 .F.,.F.,.F.)
B_SPLINE_SURFACE_WITH_KNOTS((6,1,1,1,1,1,1,1,1,1,1,1,1,1,1,1,1,1,1,1,1,
1,1,1,1,1,1,1,1,1,1,1,1,1,1,1,1,1,1,1,1,1,1,1,1,1,1,1,1,1,1,1,1,1,1,1,1,
1,1,1,1,1,1,1,1,6),(2,2),(-1.,-0.984615384615383,-0.969230769230768,-0.953846153846152,
-0.938461538461537,-0.923076923076922,-0.907692307692306,-0.892307692307691,
-0.876923076923076,-0.86153846153846,-0.846153846153845,-0.83076923076923,
-0.815384615384614,-0.799999999999999,-0.784615384615384,-0.769230769230768,
-0.753846153846153,-0.738461538461538,-0.723076923076922,-0.707692307692307,
-0.692307692307692,-0.676923076923076,-0.661538461538461,-0.646153846153846,
-0.63076923076923,-0.615384615384615,-0.6,-0.584615384615384,-0.569230769230769,
-0.553846153846154,-0.538461538461538,-0.523076923076923,-0.507692307692308,
-0.492307692307692,-0.476923076923077,-0.461538461538462,-0.446153846153846,
-0.430769230769231,-0.415384615384615,-0.4,-0.384615384615385,-0.369230769230769,
-0.353846153846154,-0.338461538461538,-0.323076923076923,-0.307692307692308,
-0.292307692307692,-0.276923076923077,-0.261538461538462,-0.246153846153846,
-0.230769230769231,-0.215384615384615,-0.2,-0.184615384615385,-0.169230769230769,
-0.153846153846154,-0.138461538461538,-0.123076923076923,-0.107692307692308,
-0.0923076923076923,-0.0769230769230769,-0.0615384615384615,-0.0461538461538462,
-0.0307692307692308,-0.0153846153846154,0.),(-1.,1.),.UNSPECIFIED.)
GEOMETRIC_REPRESENTATION_ITEM()
RATIONAL_B_SPLINE_SURFACE(((1.,1.),(1.,1.),(1.,1.),(1.,1.),(1.,1.),(1.,
1.),(1.,1.),(1.,1.),(1.,1.),(1.,1.),(1.,1.),(1.,1.),(1.,1.),(1.,1.),(1.,
1.),(1.,1.),(1.,1.),(1.,1.),(1.,1.),(1.,1.),(1.,1.),(1.,1.),(1.,1.),(1.,
1.),(1.,1.),(1.,1.),(1.,1.),(1.,1.),(1.,1.),(1.,1.),(1.,1.),(1.,1.),(1.,
1.),(1.,1.),(1.,1.),(1.,1.),(1.,1.),(1.,1.),(1.,1.),(1.,1.),(1.,1.),(1.,
1.),(1.,1.),(1.,1.),(1.,1.),(1.,1.),(1.,1.),(1.,1.),(1.,1.),(1.,1.),(1.,
1.),(1.,1.),(1.,1.),(1.,1.),(1.,1.),(1.,1.),(1.,1.),(1.,1.),(1.,1.),(1.,
1.),(1.,1.),(1.,1.),(1.,1.),(1.,1.),(1.,1.),(1.,1.),(1.,1.),(1.,1.),(1.,
1.),(1.,1.)))
REPRESENTATION_ITEM('')
SURFACE()
);
#41=(
BOUNDED_SURFACE()
B_SPLINE_SURFACE(5,1,((#30797,#30798),(#30799,#30800),(#30801,#30802),(#30803,
#30804),(#30805,#30806),(#30807,#30808),(#30809,#30810),(#30811,#30812),
(#30813,#30814),(#30815,#30816),(#30817,#30818),(#30819,#30820),(#30821,
#30822),(#30823,#30824),(#30825,#30826),(#30827,#30828),(#30829,#30830),
(#30831,#30832),(#30833,#30834),(#30835,#30836),(#30837,#30838),(#30839,
#30840),(#30841,#30842),(#30843,#30844),(#30845,#30846),(#30847,#30848),
(#30849,#30850),(#30851,#30852),(#30853,#30854),(#30855,#30856),(#30857,
#30858),(#30859,#30860),(#30861,#30862),(#30863,#30864),(#30865,#30866),
(#30867,#30868),(#30869,#30870),(#30871,#30872),(#30873,#30874),(#30875,
#30876),(#30877,#30878),(#30879,#30880),(#30881,#30882),(#30883,#30884),
(#30885,#30886),(#30887,#30888),(#30889,#30890),(#30891,#30892),(#30893,
#30894),(#30895,#30896),(#30897,#30898),(#30899,#30900),(#30901,#30902),
(#30903,#30904),(#30905,#30906),(#30907,#30908),(#30909,#30910),(#30911,
#30912),(#30913,#30914),(#30915,#30916),(#30917,#30918),(#30919,#30920),
(#30921,#30922),(#30923,#30924),(#30925,#30926),(#30927,#30928),(#30929,
#30930),(#30931,#30932),(#30933,#30934),(#30935,#30936)),.UNSPECIFIED.,
 .F.,.F.,.F.)
B_SPLINE_SURFACE_WITH_KNOTS((6,1,1,1,1,1,1,1,1,1,1,1,1,1,1,1,1,1,1,1,1,
1,1,1,1,1,1,1,1,1,1,1,1,1,1,1,1,1,1,1,1,1,1,1,1,1,1,1,1,1,1,1,1,1,1,1,1,
1,1,1,1,1,1,1,1,6),(2,2),(-1.,-0.984615384615383,-0.969230769230768,-0.953846153846152,
-0.938461538461537,-0.923076923076922,-0.907692307692306,-0.892307692307691,
-0.876923076923076,-0.86153846153846,-0.846153846153845,-0.83076923076923,
-0.815384615384614,-0.799999999999999,-0.784615384615384,-0.769230769230768,
-0.753846153846153,-0.738461538461538,-0.723076923076922,-0.707692307692307,
-0.692307692307692,-0.676923076923076,-0.661538461538461,-0.646153846153846,
-0.63076923076923,-0.615384615384615,-0.6,-0.584615384615384,-0.569230769230769,
-0.553846153846154,-0.538461538461538,-0.523076923076923,-0.507692307692308,
-0.492307692307692,-0.476923076923077,-0.461538461538462,-0.446153846153846,
-0.430769230769231,-0.415384615384615,-0.4,-0.384615384615385,-0.369230769230769,
-0.353846153846154,-0.338461538461538,-0.323076923076923,-0.307692307692308,
-0.292307692307692,-0.276923076923077,-0.261538461538462,-0.246153846153846,
-0.230769230769231,-0.215384615384615,-0.2,-0.184615384615385,-0.169230769230769,
-0.153846153846154,-0.138461538461538,-0.123076923076923,-0.107692307692308,
-0.0923076923076923,-0.0769230769230769,-0.0615384615384615,-0.0461538461538462,
-0.0307692307692308,-0.0153846153846154,0.),(-1.,1.),.UNSPECIFIED.)
GEOMETRIC_REPRESENTATION_ITEM()
RATIONAL_B_SPLINE_SURFACE(((1.,1.),(1.,1.),(1.,1.),(1.,1.),(1.,1.),(1.,
1.),(1.,1.),(1.,1.),(1.,1.),(1.,1.),(1.,1.),(1.,1.),(1.,1.),(1.,1.),(1.,
1.),(1.,1.),(1.,1.),(1.,1.),(1.,1.),(1.,1.),(1.,1.),(1.,1.),(1.,1.),(1.,
1.),(1.,1.),(1.,1.),(1.,1.),(1.,1.),(1.,1.),(1.,1.),(1.,1.),(1.,1.),(1.,
1.),(1.,1.),(1.,1.),(1.,1.),(1.,1.),(1.,1.),(1.,1.),(1.,1.),(1.,1.),(1.,
1.),(1.,1.),(1.,1.),(1.,1.),(1.,1.),(1.,1.),(1.,1.),(1.,1.),(1.,1.),(1.,
1.),(1.,1.),(1.,1.),(1.,1.),(1.,1.),(1.,1.),(1.,1.),(1.,1.),(1.,1.),(1.,
1.),(1.,1.),(1.,1.),(1.,1.),(1.,1.),(1.,1.),(1.,1.),(1.,1.),(1.,1.),(1.,
1.),(1.,1.)))
REPRESENTATION_ITEM('')
SURFACE()
);
#42=(
BOUNDED_SURFACE()
B_SPLINE_SURFACE(5,1,((#31013,#31014),(#31015,#31016),(#31017,#31018),(#31019,
#31020),(#31021,#31022),(#31023,#31024),(#31025,#31026),(#31027,#31028),
(#31029,#31030),(#31031,#31032),(#31033,#31034),(#31035,#31036),(#31037,
#31038),(#31039,#31040),(#31041,#31042),(#31043,#31044),(#31045,#31046),
(#31047,#31048),(#31049,#31050),(#31051,#31052),(#31053,#31054),(#31055,
#31056),(#31057,#31058),(#31059,#31060),(#31061,#31062),(#31063,#31064),
(#31065,#31066),(#31067,#31068),(#31069,#31070),(#31071,#31072),(#31073,
#31074),(#31075,#31076),(#31077,#31078),(#31079,#31080),(#31081,#31082),
(#31083,#31084),(#31085,#31086),(#31087,#31088),(#31089,#31090),(#31091,
#31092),(#31093,#31094),(#31095,#31096),(#31097,#31098),(#31099,#31100),
(#31101,#31102),(#31103,#31104),(#31105,#31106),(#31107,#31108),(#31109,
#31110),(#31111,#31112),(#31113,#31114),(#31115,#31116),(#31117,#31118),
(#31119,#31120),(#31121,#31122),(#31123,#31124),(#31125,#31126),(#31127,
#31128),(#31129,#31130),(#31131,#31132),(#31133,#31134),(#31135,#31136),
(#31137,#31138),(#31139,#31140),(#31141,#31142),(#31143,#31144),(#31145,
#31146),(#31147,#31148),(#31149,#31150),(#31151,#31152)),.UNSPECIFIED.,
 .F.,.F.,.F.)
B_SPLINE_SURFACE_WITH_KNOTS((6,1,1,1,1,1,1,1,1,1,1,1,1,1,1,1,1,1,1,1,1,
1,1,1,1,1,1,1,1,1,1,1,1,1,1,1,1,1,1,1,1,1,1,1,1,1,1,1,1,1,1,1,1,1,1,1,1,
1,1,1,1,1,1,1,1,6),(2,2),(-1.,-0.984615384615383,-0.969230769230768,-0.953846153846152,
-0.938461538461537,-0.923076923076922,-0.907692307692306,-0.892307692307691,
-0.876923076923076,-0.86153846153846,-0.846153846153845,-0.83076923076923,
-0.815384615384614,-0.799999999999999,-0.784615384615384,-0.769230769230768,
-0.753846153846153,-0.738461538461538,-0.723076923076922,-0.707692307692307,
-0.692307692307692,-0.676923076923076,-0.661538461538461,-0.646153846153846,
-0.63076923076923,-0.615384615384615,-0.6,-0.584615384615384,-0.569230769230769,
-0.553846153846154,-0.538461538461538,-0.523076923076923,-0.507692307692308,
-0.492307692307692,-0.476923076923077,-0.461538461538462,-0.446153846153846,
-0.430769230769231,-0.415384615384615,-0.4,-0.384615384615385,-0.369230769230769,
-0.353846153846154,-0.338461538461538,-0.323076923076923,-0.307692307692308,
-0.292307692307692,-0.276923076923077,-0.261538461538462,-0.246153846153846,
-0.230769230769231,-0.215384615384615,-0.2,-0.184615384615385,-0.169230769230769,
-0.153846153846154,-0.138461538461538,-0.123076923076923,-0.107692307692308,
-0.0923076923076923,-0.0769230769230769,-0.0615384615384615,-0.0461538461538462,
-0.0307692307692308,-0.0153846153846154,0.),(-1.,1.),.UNSPECIFIED.)
GEOMETRIC_REPRESENTATION_ITEM()
RATIONAL_B_SPLINE_SURFACE(((1.,1.),(1.,1.),(1.,1.),(1.,1.),(1.,1.),(1.,
1.),(1.,1.),(1.,1.),(1.,1.),(1.,1.),(1.,1.),(1.,1.),(1.,1.),(1.,1.),(1.,
1.),(1.,1.),(1.,1.),(1.,1.),(1.,1.),(1.,1.),(1.,1.),(1.,1.),(1.,1.),(1.,
1.),(1.,1.),(1.,1.),(1.,1.),(1.,1.),(1.,1.),(1.,1.),(1.,1.),(1.,1.),(1.,
1.),(1.,1.),(1.,1.),(1.,1.),(1.,1.),(1.,1.),(1.,1.),(1.,1.),(1.,1.),(1.,
1.),(1.,1.),(1.,1.),(1.,1.),(1.,1.),(1.,1.),(1.,1.),(1.,1.),(1.,1.),(1.,
1.),(1.,1.),(1.,1.),(1.,1.),(1.,1.),(1.,1.),(1.,1.),(1.,1.),(1.,1.),(1.,
1.),(1.,1.),(1.,1.),(1.,1.),(1.,1.),(1.,1.),(1.,1.),(1.,1.),(1.,1.),(1.,
1.),(1.,1.)))
REPRESENTATION_ITEM('')
SURFACE()
);
#43=(
BOUNDED_SURFACE()
B_SPLINE_SURFACE(5,1,((#31229,#31230),(#31231,#31232),(#31233,#31234),(#31235,
#31236),(#31237,#31238),(#31239,#31240),(#31241,#31242),(#31243,#31244),
(#31245,#31246),(#31247,#31248),(#31249,#31250),(#31251,#31252),(#31253,
#31254),(#31255,#31256),(#31257,#31258),(#31259,#31260),(#31261,#31262),
(#31263,#31264),(#31265,#31266),(#31267,#31268),(#31269,#31270),(#31271,
#31272),(#31273,#31274),(#31275,#31276),(#31277,#31278),(#31279,#31280),
(#31281,#31282),(#31283,#31284),(#31285,#31286),(#31287,#31288),(#31289,
#31290),(#31291,#31292),(#31293,#31294),(#31295,#31296),(#31297,#31298),
(#31299,#31300),(#31301,#31302),(#31303,#31304),(#31305,#31306),(#31307,
#31308),(#31309,#31310),(#31311,#31312),(#31313,#31314),(#31315,#31316),
(#31317,#31318),(#31319,#31320),(#31321,#31322),(#31323,#31324),(#31325,
#31326),(#31327,#31328),(#31329,#31330),(#31331,#31332),(#31333,#31334),
(#31335,#31336),(#31337,#31338),(#31339,#31340),(#31341,#31342),(#31343,
#31344),(#31345,#31346),(#31347,#31348),(#31349,#31350),(#31351,#31352),
(#31353,#31354),(#31355,#31356),(#31357,#31358),(#31359,#31360),(#31361,
#31362),(#31363,#31364),(#31365,#31366),(#31367,#31368)),.UNSPECIFIED.,
 .F.,.F.,.F.)
B_SPLINE_SURFACE_WITH_KNOTS((6,1,1,1,1,1,1,1,1,1,1,1,1,1,1,1,1,1,1,1,1,
1,1,1,1,1,1,1,1,1,1,1,1,1,1,1,1,1,1,1,1,1,1,1,1,1,1,1,1,1,1,1,1,1,1,1,1,
1,1,1,1,1,1,1,1,6),(2,2),(-1.,-0.984615384615383,-0.969230769230768,-0.953846153846152,
-0.938461538461537,-0.923076923076922,-0.907692307692306,-0.892307692307691,
-0.876923076923076,-0.86153846153846,-0.846153846153845,-0.83076923076923,
-0.815384615384614,-0.799999999999999,-0.784615384615384,-0.769230769230768,
-0.753846153846153,-0.738461538461538,-0.723076923076922,-0.707692307692307,
-0.692307692307692,-0.676923076923076,-0.661538461538461,-0.646153846153846,
-0.63076923076923,-0.615384615384615,-0.6,-0.584615384615384,-0.569230769230769,
-0.553846153846154,-0.538461538461538,-0.523076923076923,-0.507692307692308,
-0.492307692307692,-0.476923076923077,-0.461538461538462,-0.446153846153846,
-0.430769230769231,-0.415384615384615,-0.4,-0.384615384615385,-0.369230769230769,
-0.353846153846154,-0.338461538461538,-0.323076923076923,-0.307692307692308,
-0.292307692307692,-0.276923076923077,-0.261538461538462,-0.246153846153846,
-0.230769230769231,-0.215384615384615,-0.2,-0.184615384615385,-0.169230769230769,
-0.153846153846154,-0.138461538461538,-0.123076923076923,-0.107692307692308,
-0.0923076923076923,-0.0769230769230769,-0.0615384615384615,-0.0461538461538462,
-0.0307692307692308,-0.0153846153846154,0.),(-1.,1.),.UNSPECIFIED.)
GEOMETRIC_REPRESENTATION_ITEM()
RATIONAL_B_SPLINE_SURFACE(((1.,1.),(1.,1.),(1.,1.),(1.,1.),(1.,1.),(1.,
1.),(1.,1.),(1.,1.),(1.,1.),(1.,1.),(1.,1.),(1.,1.),(1.,1.),(1.,1.),(1.,
1.),(1.,1.),(1.,1.),(1.,1.),(1.,1.),(1.,1.),(1.,1.),(1.,1.),(1.,1.),(1.,
1.),(1.,1.),(1.,1.),(1.,1.),(1.,1.),(1.,1.),(1.,1.),(1.,1.),(1.,1.),(1.,
1.),(1.,1.),(1.,1.),(1.,1.),(1.,1.),(1.,1.),(1.,1.),(1.,1.),(1.,1.),(1.,
1.),(1.,1.),(1.,1.),(1.,1.),(1.,1.),(1.,1.),(1.,1.),(1.,1.),(1.,1.),(1.,
1.),(1.,1.),(1.,1.),(1.,1.),(1.,1.),(1.,1.),(1.,1.),(1.,1.),(1.,1.),(1.,
1.),(1.,1.),(1.,1.),(1.,1.),(1.,1.),(1.,1.),(1.,1.),(1.,1.),(1.,1.),(1.,
1.),(1.,1.)))
REPRESENTATION_ITEM('')
SURFACE()
);
#44=(
BOUNDED_SURFACE()
B_SPLINE_SURFACE(5,1,((#31445,#31446),(#31447,#31448),(#31449,#31450),(#31451,
#31452),(#31453,#31454),(#31455,#31456),(#31457,#31458),(#31459,#31460),
(#31461,#31462),(#31463,#31464),(#31465,#31466),(#31467,#31468),(#31469,
#31470),(#31471,#31472),(#31473,#31474),(#31475,#31476),(#31477,#31478),
(#31479,#31480),(#31481,#31482),(#31483,#31484),(#31485,#31486),(#31487,
#31488),(#31489,#31490),(#31491,#31492),(#31493,#31494),(#31495,#31496),
(#31497,#31498),(#31499,#31500),(#31501,#31502),(#31503,#31504),(#31505,
#31506),(#31507,#31508),(#31509,#31510),(#31511,#31512),(#31513,#31514),
(#31515,#31516),(#31517,#31518),(#31519,#31520),(#31521,#31522),(#31523,
#31524),(#31525,#31526),(#31527,#31528),(#31529,#31530),(#31531,#31532),
(#31533,#31534),(#31535,#31536),(#31537,#31538),(#31539,#31540),(#31541,
#31542),(#31543,#31544),(#31545,#31546),(#31547,#31548),(#31549,#31550),
(#31551,#31552),(#31553,#31554),(#31555,#31556),(#31557,#31558),(#31559,
#31560),(#31561,#31562),(#31563,#31564),(#31565,#31566),(#31567,#31568),
(#31569,#31570),(#31571,#31572),(#31573,#31574),(#31575,#31576),(#31577,
#31578),(#31579,#31580),(#31581,#31582),(#31583,#31584)),.UNSPECIFIED.,
 .F.,.F.,.F.)
B_SPLINE_SURFACE_WITH_KNOTS((6,1,1,1,1,1,1,1,1,1,1,1,1,1,1,1,1,1,1,1,1,
1,1,1,1,1,1,1,1,1,1,1,1,1,1,1,1,1,1,1,1,1,1,1,1,1,1,1,1,1,1,1,1,1,1,1,1,
1,1,1,1,1,1,1,1,6),(2,2),(-1.,-0.984615384615383,-0.969230769230768,-0.953846153846152,
-0.938461538461537,-0.923076923076922,-0.907692307692306,-0.892307692307691,
-0.876923076923076,-0.86153846153846,-0.846153846153845,-0.83076923076923,
-0.815384615384614,-0.799999999999999,-0.784615384615384,-0.769230769230768,
-0.753846153846153,-0.738461538461538,-0.723076923076922,-0.707692307692307,
-0.692307692307692,-0.676923076923076,-0.661538461538461,-0.646153846153846,
-0.63076923076923,-0.615384615384615,-0.6,-0.584615384615384,-0.569230769230769,
-0.553846153846154,-0.538461538461538,-0.523076923076923,-0.507692307692308,
-0.492307692307692,-0.476923076923077,-0.461538461538462,-0.446153846153846,
-0.430769230769231,-0.415384615384615,-0.4,-0.384615384615385,-0.369230769230769,
-0.353846153846154,-0.338461538461538,-0.323076923076923,-0.307692307692308,
-0.292307692307692,-0.276923076923077,-0.261538461538462,-0.246153846153846,
-0.230769230769231,-0.215384615384615,-0.2,-0.184615384615385,-0.169230769230769,
-0.153846153846154,-0.138461538461538,-0.123076923076923,-0.107692307692308,
-0.0923076923076923,-0.0769230769230769,-0.0615384615384615,-0.0461538461538462,
-0.0307692307692308,-0.0153846153846154,0.),(-1.,1.),.UNSPECIFIED.)
GEOMETRIC_REPRESENTATION_ITEM()
RATIONAL_B_SPLINE_SURFACE(((1.,1.),(1.,1.),(1.,1.),(1.,1.),(1.,1.),(1.,
1.),(1.,1.),(1.,1.),(1.,1.),(1.,1.),(1.,1.),(1.,1.),(1.,1.),(1.,1.),(1.,
1.),(1.,1.),(1.,1.),(1.,1.),(1.,1.),(1.,1.),(1.,1.),(1.,1.),(1.,1.),(1.,
1.),(1.,1.),(1.,1.),(1.,1.),(1.,1.),(1.,1.),(1.,1.),(1.,1.),(1.,1.),(1.,
1.),(1.,1.),(1.,1.),(1.,1.),(1.,1.),(1.,1.),(1.,1.),(1.,1.),(1.,1.),(1.,
1.),(1.,1.),(1.,1.),(1.,1.),(1.,1.),(1.,1.),(1.,1.),(1.,1.),(1.,1.),(1.,
1.),(1.,1.),(1.,1.),(1.,1.),(1.,1.),(1.,1.),(1.,1.),(1.,1.),(1.,1.),(1.,
1.),(1.,1.),(1.,1.),(1.,1.),(1.,1.),(1.,1.),(1.,1.),(1.,1.),(1.,1.),(1.,
1.),(1.,1.)))
REPRESENTATION_ITEM('')
SURFACE()
);
#45=(
BOUNDED_SURFACE()
B_SPLINE_SURFACE(5,1,((#31661,#31662),(#31663,#31664),(#31665,#31666),(#31667,
#31668),(#31669,#31670),(#31671,#31672),(#31673,#31674),(#31675,#31676),
(#31677,#31678),(#31679,#31680),(#31681,#31682),(#31683,#31684),(#31685,
#31686),(#31687,#31688),(#31689,#31690),(#31691,#31692),(#31693,#31694),
(#31695,#31696),(#31697,#31698),(#31699,#31700),(#31701,#31702),(#31703,
#31704),(#31705,#31706),(#31707,#31708),(#31709,#31710),(#31711,#31712),
(#31713,#31714),(#31715,#31716),(#31717,#31718),(#31719,#31720),(#31721,
#31722),(#31723,#31724),(#31725,#31726),(#31727,#31728),(#31729,#31730),
(#31731,#31732),(#31733,#31734),(#31735,#31736),(#31737,#31738),(#31739,
#31740),(#31741,#31742),(#31743,#31744),(#31745,#31746),(#31747,#31748),
(#31749,#31750),(#31751,#31752),(#31753,#31754),(#31755,#31756),(#31757,
#31758),(#31759,#31760),(#31761,#31762),(#31763,#31764),(#31765,#31766),
(#31767,#31768),(#31769,#31770),(#31771,#31772),(#31773,#31774),(#31775,
#31776),(#31777,#31778),(#31779,#31780),(#31781,#31782),(#31783,#31784),
(#31785,#31786),(#31787,#31788),(#31789,#31790),(#31791,#31792),(#31793,
#31794),(#31795,#31796),(#31797,#31798),(#31799,#31800)),.UNSPECIFIED.,
 .F.,.F.,.F.)
B_SPLINE_SURFACE_WITH_KNOTS((6,1,1,1,1,1,1,1,1,1,1,1,1,1,1,1,1,1,1,1,1,
1,1,1,1,1,1,1,1,1,1,1,1,1,1,1,1,1,1,1,1,1,1,1,1,1,1,1,1,1,1,1,1,1,1,1,1,
1,1,1,1,1,1,1,1,6),(2,2),(-1.,-0.984615384615383,-0.969230769230768,-0.953846153846152,
-0.938461538461537,-0.923076923076922,-0.907692307692306,-0.892307692307691,
-0.876923076923076,-0.86153846153846,-0.846153846153845,-0.83076923076923,
-0.815384615384614,-0.799999999999999,-0.784615384615384,-0.769230769230768,
-0.753846153846153,-0.738461538461538,-0.723076923076922,-0.707692307692307,
-0.692307692307692,-0.676923076923076,-0.661538461538461,-0.646153846153846,
-0.63076923076923,-0.615384615384615,-0.6,-0.584615384615384,-0.569230769230769,
-0.553846153846154,-0.538461538461538,-0.523076923076923,-0.507692307692308,
-0.492307692307692,-0.476923076923077,-0.461538461538462,-0.446153846153846,
-0.430769230769231,-0.415384615384615,-0.4,-0.384615384615385,-0.369230769230769,
-0.353846153846154,-0.338461538461538,-0.323076923076923,-0.307692307692308,
-0.292307692307692,-0.276923076923077,-0.261538461538462,-0.246153846153846,
-0.230769230769231,-0.215384615384615,-0.2,-0.184615384615385,-0.169230769230769,
-0.153846153846154,-0.138461538461538,-0.123076923076923,-0.107692307692308,
-0.0923076923076923,-0.0769230769230769,-0.0615384615384615,-0.0461538461538462,
-0.0307692307692308,-0.0153846153846154,0.),(-1.,1.),.UNSPECIFIED.)
GEOMETRIC_REPRESENTATION_ITEM()
RATIONAL_B_SPLINE_SURFACE(((1.,1.),(1.,1.),(1.,1.),(1.,1.),(1.,1.),(1.,
1.),(1.,1.),(1.,1.),(1.,1.),(1.,1.),(1.,1.),(1.,1.),(1.,1.),(1.,1.),(1.,
1.),(1.,1.),(1.,1.),(1.,1.),(1.,1.),(1.,1.),(1.,1.),(1.,1.),(1.,1.),(1.,
1.),(1.,1.),(1.,1.),(1.,1.),(1.,1.),(1.,1.),(1.,1.),(1.,1.),(1.,1.),(1.,
1.),(1.,1.),(1.,1.),(1.,1.),(1.,1.),(1.,1.),(1.,1.),(1.,1.),(1.,1.),(1.,
1.),(1.,1.),(1.,1.),(1.,1.),(1.,1.),(1.,1.),(1.,1.),(1.,1.),(1.,1.),(1.,
1.),(1.,1.),(1.,1.),(1.,1.),(1.,1.),(1.,1.),(1.,1.),(1.,1.),(1.,1.),(1.,
1.),(1.,1.),(1.,1.),(1.,1.),(1.,1.),(1.,1.),(1.,1.),(1.,1.),(1.,1.),(1.,
1.),(1.,1.)))
REPRESENTATION_ITEM('')
SURFACE()
);
#46=(
BOUNDED_SURFACE()
B_SPLINE_SURFACE(5,1,((#31877,#31878),(#31879,#31880),(#31881,#31882),(#31883,
#31884),(#31885,#31886),(#31887,#31888),(#31889,#31890),(#31891,#31892),
(#31893,#31894),(#31895,#31896),(#31897,#31898),(#31899,#31900),(#31901,
#31902),(#31903,#31904),(#31905,#31906),(#31907,#31908),(#31909,#31910),
(#31911,#31912),(#31913,#31914),(#31915,#31916),(#31917,#31918),(#31919,
#31920),(#31921,#31922),(#31923,#31924),(#31925,#31926),(#31927,#31928),
(#31929,#31930),(#31931,#31932),(#31933,#31934),(#31935,#31936),(#31937,
#31938),(#31939,#31940),(#31941,#31942),(#31943,#31944),(#31945,#31946),
(#31947,#31948),(#31949,#31950),(#31951,#31952),(#31953,#31954),(#31955,
#31956),(#31957,#31958),(#31959,#31960),(#31961,#31962),(#31963,#31964),
(#31965,#31966),(#31967,#31968),(#31969,#31970),(#31971,#31972),(#31973,
#31974),(#31975,#31976),(#31977,#31978),(#31979,#31980),(#31981,#31982),
(#31983,#31984),(#31985,#31986),(#31987,#31988),(#31989,#31990),(#31991,
#31992),(#31993,#31994),(#31995,#31996),(#31997,#31998),(#31999,#32000),
(#32001,#32002),(#32003,#32004),(#32005,#32006),(#32007,#32008),(#32009,
#32010),(#32011,#32012),(#32013,#32014),(#32015,#32016)),.UNSPECIFIED.,
 .F.,.F.,.F.)
B_SPLINE_SURFACE_WITH_KNOTS((6,1,1,1,1,1,1,1,1,1,1,1,1,1,1,1,1,1,1,1,1,
1,1,1,1,1,1,1,1,1,1,1,1,1,1,1,1,1,1,1,1,1,1,1,1,1,1,1,1,1,1,1,1,1,1,1,1,
1,1,1,1,1,1,1,1,6),(2,2),(-1.,-0.984615384615383,-0.969230769230768,-0.953846153846152,
-0.938461538461537,-0.923076923076922,-0.907692307692306,-0.892307692307691,
-0.876923076923076,-0.86153846153846,-0.846153846153845,-0.83076923076923,
-0.815384615384614,-0.799999999999999,-0.784615384615384,-0.769230769230768,
-0.753846153846153,-0.738461538461538,-0.723076923076922,-0.707692307692307,
-0.692307692307692,-0.676923076923076,-0.661538461538461,-0.646153846153846,
-0.63076923076923,-0.615384615384615,-0.6,-0.584615384615384,-0.569230769230769,
-0.553846153846154,-0.538461538461538,-0.523076923076923,-0.507692307692308,
-0.492307692307692,-0.476923076923077,-0.461538461538462,-0.446153846153846,
-0.430769230769231,-0.415384615384615,-0.4,-0.384615384615385,-0.369230769230769,
-0.353846153846154,-0.338461538461538,-0.323076923076923,-0.307692307692308,
-0.292307692307692,-0.276923076923077,-0.261538461538462,-0.246153846153846,
-0.230769230769231,-0.215384615384615,-0.2,-0.184615384615385,-0.169230769230769,
-0.153846153846154,-0.138461538461538,-0.123076923076923,-0.107692307692308,
-0.0923076923076923,-0.0769230769230769,-0.0615384615384615,-0.0461538461538462,
-0.0307692307692308,-0.0153846153846154,0.),(-1.,1.),.UNSPECIFIED.)
GEOMETRIC_REPRESENTATION_ITEM()
RATIONAL_B_SPLINE_SURFACE(((1.,1.),(1.,1.),(1.,1.),(1.,1.),(1.,1.),(1.,
1.),(1.,1.),(1.,1.),(1.,1.),(1.,1.),(1.,1.),(1.,1.),(1.,1.),(1.,1.),(1.,
1.),(1.,1.),(1.,1.),(1.,1.),(1.,1.),(1.,1.),(1.,1.),(1.,1.),(1.,1.),(1.,
1.),(1.,1.),(1.,1.),(1.,1.),(1.,1.),(1.,1.),(1.,1.),(1.,1.),(1.,1.),(1.,
1.),(1.,1.),(1.,1.),(1.,1.),(1.,1.),(1.,1.),(1.,1.),(1.,1.),(1.,1.),(1.,
1.),(1.,1.),(1.,1.),(1.,1.),(1.,1.),(1.,1.),(1.,1.),(1.,1.),(1.,1.),(1.,
1.),(1.,1.),(1.,1.),(1.,1.),(1.,1.),(1.,1.),(1.,1.),(1.,1.),(1.,1.),(1.,
1.),(1.,1.),(1.,1.),(1.,1.),(1.,1.),(1.,1.),(1.,1.),(1.,1.),(1.,1.),(1.,
1.),(1.,1.)))
REPRESENTATION_ITEM('')
SURFACE()
);
#47=(
BOUNDED_SURFACE()
B_SPLINE_SURFACE(5,1,((#32093,#32094),(#32095,#32096),(#32097,#32098),(#32099,
#32100),(#32101,#32102),(#32103,#32104),(#32105,#32106),(#32107,#32108),
(#32109,#32110),(#32111,#32112),(#32113,#32114),(#32115,#32116),(#32117,
#32118),(#32119,#32120),(#32121,#32122),(#32123,#32124),(#32125,#32126),
(#32127,#32128),(#32129,#32130),(#32131,#32132),(#32133,#32134),(#32135,
#32136),(#32137,#32138),(#32139,#32140),(#32141,#32142),(#32143,#32144),
(#32145,#32146),(#32147,#32148),(#32149,#32150),(#32151,#32152),(#32153,
#32154),(#32155,#32156),(#32157,#32158),(#32159,#32160),(#32161,#32162),
(#32163,#32164),(#32165,#32166),(#32167,#32168),(#32169,#32170),(#32171,
#32172),(#32173,#32174),(#32175,#32176),(#32177,#32178),(#32179,#32180),
(#32181,#32182),(#32183,#32184),(#32185,#32186),(#32187,#32188),(#32189,
#32190),(#32191,#32192),(#32193,#32194),(#32195,#32196),(#32197,#32198),
(#32199,#32200),(#32201,#32202),(#32203,#32204),(#32205,#32206),(#32207,
#32208),(#32209,#32210),(#32211,#32212),(#32213,#32214),(#32215,#32216),
(#32217,#32218),(#32219,#32220),(#32221,#32222),(#32223,#32224),(#32225,
#32226),(#32227,#32228),(#32229,#32230),(#32231,#32232)),.UNSPECIFIED.,
 .F.,.F.,.F.)
B_SPLINE_SURFACE_WITH_KNOTS((6,1,1,1,1,1,1,1,1,1,1,1,1,1,1,1,1,1,1,1,1,
1,1,1,1,1,1,1,1,1,1,1,1,1,1,1,1,1,1,1,1,1,1,1,1,1,1,1,1,1,1,1,1,1,1,1,1,
1,1,1,1,1,1,1,1,6),(2,2),(-1.,-0.984615384615383,-0.969230769230768,-0.953846153846152,
-0.938461538461537,-0.923076923076922,-0.907692307692306,-0.892307692307691,
-0.876923076923076,-0.86153846153846,-0.846153846153845,-0.83076923076923,
-0.815384615384614,-0.799999999999999,-0.784615384615384,-0.769230769230768,
-0.753846153846153,-0.738461538461538,-0.723076923076922,-0.707692307692307,
-0.692307692307692,-0.676923076923076,-0.661538461538461,-0.646153846153846,
-0.63076923076923,-0.615384615384615,-0.6,-0.584615384615384,-0.569230769230769,
-0.553846153846154,-0.538461538461538,-0.523076923076923,-0.507692307692308,
-0.492307692307692,-0.476923076923077,-0.461538461538462,-0.446153846153846,
-0.430769230769231,-0.415384615384615,-0.4,-0.384615384615385,-0.369230769230769,
-0.353846153846154,-0.338461538461538,-0.323076923076923,-0.307692307692308,
-0.292307692307692,-0.276923076923077,-0.261538461538462,-0.246153846153846,
-0.230769230769231,-0.215384615384615,-0.2,-0.184615384615385,-0.169230769230769,
-0.153846153846154,-0.138461538461538,-0.123076923076923,-0.107692307692308,
-0.0923076923076923,-0.0769230769230769,-0.0615384615384615,-0.0461538461538462,
-0.0307692307692308,-0.0153846153846154,0.),(-1.,1.),.UNSPECIFIED.)
GEOMETRIC_REPRESENTATION_ITEM()
RATIONAL_B_SPLINE_SURFACE(((1.,1.),(1.,1.),(1.,1.),(1.,1.),(1.,1.),(1.,
1.),(1.,1.),(1.,1.),(1.,1.),(1.,1.),(1.,1.),(1.,1.),(1.,1.),(1.,1.),(1.,
1.),(1.,1.),(1.,1.),(1.,1.),(1.,1.),(1.,1.),(1.,1.),(1.,1.),(1.,1.),(1.,
1.),(1.,1.),(1.,1.),(1.,1.),(1.,1.),(1.,1.),(1.,1.),(1.,1.),(1.,1.),(1.,
1.),(1.,1.),(1.,1.),(1.,1.),(1.,1.),(1.,1.),(1.,1.),(1.,1.),(1.,1.),(1.,
1.),(1.,1.),(1.,1.),(1.,1.),(1.,1.),(1.,1.),(1.,1.),(1.,1.),(1.,1.),(1.,
1.),(1.,1.),(1.,1.),(1.,1.),(1.,1.),(1.,1.),(1.,1.),(1.,1.),(1.,1.),(1.,
1.),(1.,1.),(1.,1.),(1.,1.),(1.,1.),(1.,1.),(1.,1.),(1.,1.),(1.,1.),(1.,
1.),(1.,1.)))
REPRESENTATION_ITEM('')
SURFACE()
);
#48=(
BOUNDED_SURFACE()
B_SPLINE_SURFACE(5,1,((#32309,#32310),(#32311,#32312),(#32313,#32314),(#32315,
#32316),(#32317,#32318),(#32319,#32320),(#32321,#32322),(#32323,#32324),
(#32325,#32326),(#32327,#32328),(#32329,#32330),(#32331,#32332),(#32333,
#32334),(#32335,#32336),(#32337,#32338),(#32339,#32340),(#32341,#32342),
(#32343,#32344),(#32345,#32346),(#32347,#32348),(#32349,#32350),(#32351,
#32352),(#32353,#32354),(#32355,#32356),(#32357,#32358),(#32359,#32360),
(#32361,#32362),(#32363,#32364),(#32365,#32366),(#32367,#32368),(#32369,
#32370),(#32371,#32372),(#32373,#32374),(#32375,#32376),(#32377,#32378),
(#32379,#32380),(#32381,#32382),(#32383,#32384),(#32385,#32386),(#32387,
#32388),(#32389,#32390),(#32391,#32392),(#32393,#32394),(#32395,#32396),
(#32397,#32398),(#32399,#32400),(#32401,#32402),(#32403,#32404),(#32405,
#32406),(#32407,#32408),(#32409,#32410),(#32411,#32412),(#32413,#32414),
(#32415,#32416),(#32417,#32418),(#32419,#32420),(#32421,#32422),(#32423,
#32424),(#32425,#32426),(#32427,#32428),(#32429,#32430),(#32431,#32432),
(#32433,#32434),(#32435,#32436),(#32437,#32438),(#32439,#32440),(#32441,
#32442),(#32443,#32444),(#32445,#32446),(#32447,#32448)),.UNSPECIFIED.,
 .F.,.F.,.F.)
B_SPLINE_SURFACE_WITH_KNOTS((6,1,1,1,1,1,1,1,1,1,1,1,1,1,1,1,1,1,1,1,1,
1,1,1,1,1,1,1,1,1,1,1,1,1,1,1,1,1,1,1,1,1,1,1,1,1,1,1,1,1,1,1,1,1,1,1,1,
1,1,1,1,1,1,1,1,6),(2,2),(-1.,-0.984615384615383,-0.969230769230768,-0.953846153846152,
-0.938461538461537,-0.923076923076922,-0.907692307692306,-0.892307692307691,
-0.876923076923076,-0.86153846153846,-0.846153846153845,-0.83076923076923,
-0.815384615384614,-0.799999999999999,-0.784615384615384,-0.769230769230768,
-0.753846153846153,-0.738461538461538,-0.723076923076922,-0.707692307692307,
-0.692307692307692,-0.676923076923076,-0.661538461538461,-0.646153846153846,
-0.63076923076923,-0.615384615384615,-0.6,-0.584615384615384,-0.569230769230769,
-0.553846153846154,-0.538461538461538,-0.523076923076923,-0.507692307692308,
-0.492307692307692,-0.476923076923077,-0.461538461538462,-0.446153846153846,
-0.430769230769231,-0.415384615384615,-0.4,-0.384615384615385,-0.369230769230769,
-0.353846153846154,-0.338461538461538,-0.323076923076923,-0.307692307692308,
-0.292307692307692,-0.276923076923077,-0.261538461538462,-0.246153846153846,
-0.230769230769231,-0.215384615384615,-0.2,-0.184615384615385,-0.169230769230769,
-0.153846153846154,-0.138461538461538,-0.123076923076923,-0.107692307692308,
-0.0923076923076923,-0.0769230769230769,-0.0615384615384615,-0.0461538461538462,
-0.0307692307692308,-0.0153846153846154,0.),(-1.,1.),.UNSPECIFIED.)
GEOMETRIC_REPRESENTATION_ITEM()
RATIONAL_B_SPLINE_SURFACE(((1.,1.),(1.,1.),(1.,1.),(1.,1.),(1.,1.),(1.,
1.),(1.,1.),(1.,1.),(1.,1.),(1.,1.),(1.,1.),(1.,1.),(1.,1.),(1.,1.),(1.,
1.),(1.,1.),(1.,1.),(1.,1.),(1.,1.),(1.,1.),(1.,1.),(1.,1.),(1.,1.),(1.,
1.),(1.,1.),(1.,1.),(1.,1.),(1.,1.),(1.,1.),(1.,1.),(1.,1.),(1.,1.),(1.,
1.),(1.,1.),(1.,1.),(1.,1.),(1.,1.),(1.,1.),(1.,1.),(1.,1.),(1.,1.),(1.,
1.),(1.,1.),(1.,1.),(1.,1.),(1.,1.),(1.,1.),(1.,1.),(1.,1.),(1.,1.),(1.,
1.),(1.,1.),(1.,1.),(1.,1.),(1.,1.),(1.,1.),(1.,1.),(1.,1.),(1.,1.),(1.,
1.),(1.,1.),(1.,1.),(1.,1.),(1.,1.),(1.,1.),(1.,1.),(1.,1.),(1.,1.),(1.,
1.),(1.,1.)))
REPRESENTATION_ITEM('')
SURFACE()
);
#49=(
BOUNDED_SURFACE()
B_SPLINE_SURFACE(5,1,((#32525,#32526),(#32527,#32528),(#32529,#32530),(#32531,
#32532),(#32533,#32534),(#32535,#32536),(#32537,#32538),(#32539,#32540),
(#32541,#32542),(#32543,#32544),(#32545,#32546),(#32547,#32548),(#32549,
#32550),(#32551,#32552),(#32553,#32554),(#32555,#32556),(#32557,#32558),
(#32559,#32560),(#32561,#32562),(#32563,#32564),(#32565,#32566),(#32567,
#32568),(#32569,#32570),(#32571,#32572),(#32573,#32574),(#32575,#32576),
(#32577,#32578),(#32579,#32580),(#32581,#32582),(#32583,#32584),(#32585,
#32586),(#32587,#32588),(#32589,#32590),(#32591,#32592),(#32593,#32594),
(#32595,#32596),(#32597,#32598),(#32599,#32600),(#32601,#32602),(#32603,
#32604),(#32605,#32606),(#32607,#32608),(#32609,#32610),(#32611,#32612),
(#32613,#32614),(#32615,#32616),(#32617,#32618),(#32619,#32620),(#32621,
#32622),(#32623,#32624),(#32625,#32626),(#32627,#32628),(#32629,#32630),
(#32631,#32632),(#32633,#32634),(#32635,#32636),(#32637,#32638),(#32639,
#32640),(#32641,#32642),(#32643,#32644),(#32645,#32646),(#32647,#32648),
(#32649,#32650),(#32651,#32652),(#32653,#32654),(#32655,#32656),(#32657,
#32658),(#32659,#32660),(#32661,#32662),(#32663,#32664)),.UNSPECIFIED.,
 .F.,.F.,.F.)
B_SPLINE_SURFACE_WITH_KNOTS((6,1,1,1,1,1,1,1,1,1,1,1,1,1,1,1,1,1,1,1,1,
1,1,1,1,1,1,1,1,1,1,1,1,1,1,1,1,1,1,1,1,1,1,1,1,1,1,1,1,1,1,1,1,1,1,1,1,
1,1,1,1,1,1,1,1,6),(2,2),(-1.,-0.984615384615383,-0.969230769230768,-0.953846153846152,
-0.938461538461537,-0.923076923076922,-0.907692307692306,-0.892307692307691,
-0.876923076923076,-0.86153846153846,-0.846153846153845,-0.83076923076923,
-0.815384615384614,-0.799999999999999,-0.784615384615384,-0.769230769230768,
-0.753846153846153,-0.738461538461538,-0.723076923076922,-0.707692307692307,
-0.692307692307692,-0.676923076923076,-0.661538461538461,-0.646153846153846,
-0.63076923076923,-0.615384615384615,-0.6,-0.584615384615384,-0.569230769230769,
-0.553846153846154,-0.538461538461538,-0.523076923076923,-0.507692307692308,
-0.492307692307692,-0.476923076923077,-0.461538461538462,-0.446153846153846,
-0.430769230769231,-0.415384615384615,-0.4,-0.384615384615385,-0.369230769230769,
-0.353846153846154,-0.338461538461538,-0.323076923076923,-0.307692307692308,
-0.292307692307692,-0.276923076923077,-0.261538461538462,-0.246153846153846,
-0.230769230769231,-0.215384615384615,-0.2,-0.184615384615385,-0.169230769230769,
-0.153846153846154,-0.138461538461538,-0.123076923076923,-0.107692307692308,
-0.0923076923076923,-0.0769230769230769,-0.0615384615384615,-0.0461538461538462,
-0.0307692307692308,-0.0153846153846154,0.),(-1.,1.),.UNSPECIFIED.)
GEOMETRIC_REPRESENTATION_ITEM()
RATIONAL_B_SPLINE_SURFACE(((1.,1.),(1.,1.),(1.,1.),(1.,1.),(1.,1.),(1.,
1.),(1.,1.),(1.,1.),(1.,1.),(1.,1.),(1.,1.),(1.,1.),(1.,1.),(1.,1.),(1.,
1.),(1.,1.),(1.,1.),(1.,1.),(1.,1.),(1.,1.),(1.,1.),(1.,1.),(1.,1.),(1.,
1.),(1.,1.),(1.,1.),(1.,1.),(1.,1.),(1.,1.),(1.,1.),(1.,1.),(1.,1.),(1.,
1.),(1.,1.),(1.,1.),(1.,1.),(1.,1.),(1.,1.),(1.,1.),(1.,1.),(1.,1.),(1.,
1.),(1.,1.),(1.,1.),(1.,1.),(1.,1.),(1.,1.),(1.,1.),(1.,1.),(1.,1.),(1.,
1.),(1.,1.),(1.,1.),(1.,1.),(1.,1.),(1.,1.),(1.,1.),(1.,1.),(1.,1.),(1.,
1.),(1.,1.),(1.,1.),(1.,1.),(1.,1.),(1.,1.),(1.,1.),(1.,1.),(1.,1.),(1.,
1.),(1.,1.)))
REPRESENTATION_ITEM('')
SURFACE()
);
#50=(
BOUNDED_SURFACE()
B_SPLINE_SURFACE(5,1,((#32741,#32742),(#32743,#32744),(#32745,#32746),(#32747,
#32748),(#32749,#32750),(#32751,#32752),(#32753,#32754),(#32755,#32756),
(#32757,#32758),(#32759,#32760),(#32761,#32762),(#32763,#32764),(#32765,
#32766),(#32767,#32768),(#32769,#32770),(#32771,#32772),(#32773,#32774),
(#32775,#32776),(#32777,#32778),(#32779,#32780),(#32781,#32782),(#32783,
#32784),(#32785,#32786),(#32787,#32788),(#32789,#32790),(#32791,#32792),
(#32793,#32794),(#32795,#32796),(#32797,#32798),(#32799,#32800),(#32801,
#32802),(#32803,#32804),(#32805,#32806),(#32807,#32808),(#32809,#32810),
(#32811,#32812),(#32813,#32814),(#32815,#32816),(#32817,#32818),(#32819,
#32820),(#32821,#32822),(#32823,#32824),(#32825,#32826),(#32827,#32828),
(#32829,#32830),(#32831,#32832),(#32833,#32834),(#32835,#32836),(#32837,
#32838),(#32839,#32840),(#32841,#32842),(#32843,#32844),(#32845,#32846),
(#32847,#32848),(#32849,#32850),(#32851,#32852),(#32853,#32854),(#32855,
#32856),(#32857,#32858),(#32859,#32860),(#32861,#32862),(#32863,#32864),
(#32865,#32866),(#32867,#32868),(#32869,#32870),(#32871,#32872),(#32873,
#32874),(#32875,#32876),(#32877,#32878),(#32879,#32880)),.UNSPECIFIED.,
 .F.,.F.,.F.)
B_SPLINE_SURFACE_WITH_KNOTS((6,1,1,1,1,1,1,1,1,1,1,1,1,1,1,1,1,1,1,1,1,
1,1,1,1,1,1,1,1,1,1,1,1,1,1,1,1,1,1,1,1,1,1,1,1,1,1,1,1,1,1,1,1,1,1,1,1,
1,1,1,1,1,1,1,1,6),(2,2),(-1.,-0.984615384615383,-0.969230769230768,-0.953846153846152,
-0.938461538461537,-0.923076923076922,-0.907692307692306,-0.892307692307691,
-0.876923076923076,-0.86153846153846,-0.846153846153845,-0.83076923076923,
-0.815384615384614,-0.799999999999999,-0.784615384615384,-0.769230769230768,
-0.753846153846153,-0.738461538461538,-0.723076923076922,-0.707692307692307,
-0.692307692307692,-0.676923076923076,-0.661538461538461,-0.646153846153846,
-0.63076923076923,-0.615384615384615,-0.6,-0.584615384615384,-0.569230769230769,
-0.553846153846154,-0.538461538461538,-0.523076923076923,-0.507692307692308,
-0.492307692307692,-0.476923076923077,-0.461538461538462,-0.446153846153846,
-0.430769230769231,-0.415384615384615,-0.4,-0.384615384615385,-0.369230769230769,
-0.353846153846154,-0.338461538461538,-0.323076923076923,-0.307692307692308,
-0.292307692307692,-0.276923076923077,-0.261538461538462,-0.246153846153846,
-0.230769230769231,-0.215384615384615,-0.2,-0.184615384615385,-0.169230769230769,
-0.153846153846154,-0.138461538461538,-0.123076923076923,-0.107692307692308,
-0.0923076923076923,-0.0769230769230769,-0.0615384615384615,-0.0461538461538462,
-0.0307692307692308,-0.0153846153846154,0.),(-1.,1.),.UNSPECIFIED.)
GEOMETRIC_REPRESENTATION_ITEM()
RATIONAL_B_SPLINE_SURFACE(((1.,1.),(1.,1.),(1.,1.),(1.,1.),(1.,1.),(1.,
1.),(1.,1.),(1.,1.),(1.,1.),(1.,1.),(1.,1.),(1.,1.),(1.,1.),(1.,1.),(1.,
1.),(1.,1.),(1.,1.),(1.,1.),(1.,1.),(1.,1.),(1.,1.),(1.,1.),(1.,1.),(1.,
1.),(1.,1.),(1.,1.),(1.,1.),(1.,1.),(1.,1.),(1.,1.),(1.,1.),(1.,1.),(1.,
1.),(1.,1.),(1.,1.),(1.,1.),(1.,1.),(1.,1.),(1.,1.),(1.,1.),(1.,1.),(1.,
1.),(1.,1.),(1.,1.),(1.,1.),(1.,1.),(1.,1.),(1.,1.),(1.,1.),(1.,1.),(1.,
1.),(1.,1.),(1.,1.),(1.,1.),(1.,1.),(1.,1.),(1.,1.),(1.,1.),(1.,1.),(1.,
1.),(1.,1.),(1.,1.),(1.,1.),(1.,1.),(1.,1.),(1.,1.),(1.,1.),(1.,1.),(1.,
1.),(1.,1.)))
REPRESENTATION_ITEM('')
SURFACE()
);
#51=(
BOUNDED_CURVE()
B_SPLINE_CURVE(5,(#21389,#21390,#21391,#21392,#21393,#21394,#21395,#21396,
#21397,#21398,#21399,#21400,#21401,#21402,#21403,#21404,#21405,#21406,#21407,
#21408,#21409,#21410,#21411,#21412,#21413,#21414,#21415,#21416,#21417,#21418,
#21419,#21420,#21421,#21422,#21423,#21424,#21425,#21426,#21427,#21428,#21429,
#21430,#21431,#21432,#21433,#21434,#21435,#21436,#21437,#21438,#21439,#21440,
#21441,#21442,#21443,#21444,#21445,#21446,#21447,#21448,#21449,#21450,#21451,
#21452,#21453,#21454,#21455,#21456,#21457,#21458),.UNSPECIFIED.,.F.,.F.)
B_SPLINE_CURVE_WITH_KNOTS((6,1,1,1,1,1,1,1,1,1,1,1,1,1,1,1,1,1,1,1,1,1,
1,1,1,1,1,1,1,1,1,1,1,1,1,1,1,1,1,1,1,1,1,1,1,1,1,1,1,1,1,1,1,1,1,1,1,1,
1,1,1,1,1,1,1,6),(0.,0.0153846153846154,0.0307692307692308,0.0461538461538462,
0.0615384615384615,0.0769230769230769,0.0923076923076923,0.107692307692308,
0.123076923076923,0.138461538461538,0.153846153846154,0.169230769230769,
0.184615384615385,0.2,0.215384615384615,0.230769230769231,0.246153846153846,
0.261538461538462,0.276923076923077,0.292307692307692,0.307692307692308,
0.323076923076923,0.338461538461538,0.353846153846154,0.369230769230769,
0.384615384615385,0.4,0.415384615384615,0.430769230769231,0.446153846153846,
0.461538461538462,0.476923076923077,0.492307692307692,0.507692307692308,
0.523076923076923,0.538461538461538,0.553846153846154,0.569230769230769,
0.584615384615384,0.6,0.615384615384615,0.63076923076923,0.646153846153846,
0.661538461538461,0.676923076923076,0.692307692307692,0.707692307692307,
0.723076923076922,0.738461538461538,0.753846153846153,0.769230769230768,
0.784615384615384,0.799999999999999,0.815384615384614,0.83076923076923,
0.846153846153845,0.86153846153846,0.876923076923076,0.892307692307691,
0.907692307692306,0.923076923076922,0.938461538461537,0.953846153846152,
0.969230769230768,0.984615384615383,1.),.UNSPECIFIED.)
CURVE()
GEOMETRIC_REPRESENTATION_ITEM()
RATIONAL_B_SPLINE_CURVE((1.,1.,1.,1.,1.,1.,1.,1.,1.,1.,1.,1.,1.,1.,1.,1.,
1.,1.,1.,1.,1.,1.,1.,1.,1.,1.,1.,1.,1.,1.,1.,1.,1.,1.,1.,1.,1.,1.,1.,1.,
1.,1.,1.,1.,1.,1.,1.,1.,1.,1.,1.,1.,1.,1.,1.,1.,1.,1.,1.,1.,1.,1.,1.,1.,
1.,1.,1.,1.,1.,1.))
REPRESENTATION_ITEM('')
);
#52=(
BOUNDED_CURVE()
B_SPLINE_CURVE(5,(#21462,#21463,#21464,#21465,#21466,#21467,#21468,#21469,
#21470,#21471,#21472,#21473,#21474,#21475,#21476,#21477,#21478,#21479,#21480,
#21481,#21482,#21483,#21484,#21485,#21486,#21487,#21488,#21489,#21490,#21491,
#21492,#21493,#21494,#21495,#21496,#21497,#21498,#21499,#21500,#21501,#21502,
#21503,#21504,#21505,#21506,#21507,#21508,#21509,#21510,#21511,#21512,#21513,
#21514,#21515,#21516,#21517,#21518,#21519,#21520,#21521,#21522,#21523,#21524,
#21525,#21526,#21527,#21528,#21529,#21530,#21531),.UNSPECIFIED.,.F.,.F.)
B_SPLINE_CURVE_WITH_KNOTS((6,1,1,1,1,1,1,1,1,1,1,1,1,1,1,1,1,1,1,1,1,1,
1,1,1,1,1,1,1,1,1,1,1,1,1,1,1,1,1,1,1,1,1,1,1,1,1,1,1,1,1,1,1,1,1,1,1,1,
1,1,1,1,1,1,1,6),(0.,0.0153846153846154,0.0307692307692308,0.0461538461538462,
0.0615384615384615,0.0769230769230769,0.0923076923076923,0.107692307692308,
0.123076923076923,0.138461538461538,0.153846153846154,0.169230769230769,
0.184615384615385,0.2,0.215384615384615,0.230769230769231,0.246153846153846,
0.261538461538462,0.276923076923077,0.292307692307692,0.307692307692308,
0.323076923076923,0.338461538461538,0.353846153846154,0.369230769230769,
0.384615384615385,0.4,0.415384615384615,0.430769230769231,0.446153846153846,
0.461538461538462,0.476923076923077,0.492307692307692,0.507692307692308,
0.523076923076923,0.538461538461538,0.553846153846154,0.569230769230769,
0.584615384615384,0.6,0.615384615384615,0.63076923076923,0.646153846153846,
0.661538461538461,0.676923076923076,0.692307692307692,0.707692307692307,
0.723076923076922,0.738461538461538,0.753846153846153,0.769230769230768,
0.784615384615384,0.799999999999999,0.815384615384614,0.83076923076923,
0.846153846153845,0.86153846153846,0.876923076923076,0.892307692307691,
0.907692307692306,0.923076923076922,0.938461538461537,0.953846153846152,
0.969230769230768,0.984615384615383,1.),.UNSPECIFIED.)
CURVE()
GEOMETRIC_REPRESENTATION_ITEM()
RATIONAL_B_SPLINE_CURVE((1.,1.,1.,1.,1.,1.,1.,1.,1.,1.,1.,1.,1.,1.,1.,1.,
1.,1.,1.,1.,1.,1.,1.,1.,1.,1.,1.,1.,1.,1.,1.,1.,1.,1.,1.,1.,1.,1.,1.,1.,
1.,1.,1.,1.,1.,1.,1.,1.,1.,1.,1.,1.,1.,1.,1.,1.,1.,1.,1.,1.,1.,1.,1.,1.,
1.,1.,1.,1.,1.,1.))
REPRESENTATION_ITEM('')
);
#53=(
BOUNDED_CURVE()
B_SPLINE_CURVE(5,(#21535,#21536,#21537,#21538,#21539,#21540,#21541,#21542,
#21543,#21544,#21545,#21546,#21547,#21548,#21549,#21550,#21551,#21552,#21553,
#21554,#21555,#21556,#21557,#21558,#21559,#21560,#21561,#21562,#21563,#21564,
#21565,#21566,#21567,#21568,#21569,#21570,#21571,#21572,#21573,#21574,#21575,
#21576,#21577,#21578,#21579,#21580,#21581,#21582,#21583,#21584,#21585,#21586,
#21587,#21588,#21589,#21590,#21591,#21592,#21593,#21594,#21595,#21596,#21597,
#21598,#21599,#21600,#21601,#21602,#21603,#21604),.UNSPECIFIED.,.F.,.F.)
B_SPLINE_CURVE_WITH_KNOTS((6,1,1,1,1,1,1,1,1,1,1,1,1,1,1,1,1,1,1,1,1,1,
1,1,1,1,1,1,1,1,1,1,1,1,1,1,1,1,1,1,1,1,1,1,1,1,1,1,1,1,1,1,1,1,1,1,1,1,
1,1,1,1,1,1,1,6),(0.,0.0153846153846154,0.0307692307692308,0.0461538461538462,
0.0615384615384615,0.0769230769230769,0.0923076923076923,0.107692307692308,
0.123076923076923,0.138461538461538,0.153846153846154,0.169230769230769,
0.184615384615385,0.2,0.215384615384615,0.230769230769231,0.246153846153846,
0.261538461538462,0.276923076923077,0.292307692307692,0.307692307692308,
0.323076923076923,0.338461538461538,0.353846153846154,0.369230769230769,
0.384615384615385,0.4,0.415384615384615,0.430769230769231,0.446153846153846,
0.461538461538462,0.476923076923077,0.492307692307692,0.507692307692308,
0.523076923076923,0.538461538461538,0.553846153846154,0.569230769230769,
0.584615384615384,0.6,0.615384615384615,0.63076923076923,0.646153846153846,
0.661538461538461,0.676923076923076,0.692307692307692,0.707692307692307,
0.723076923076922,0.738461538461538,0.753846153846153,0.769230769230768,
0.784615384615384,0.799999999999999,0.815384615384614,0.83076923076923,
0.846153846153845,0.86153846153846,0.876923076923076,0.892307692307691,
0.907692307692306,0.923076923076922,0.938461538461537,0.953846153846152,
0.969230769230768,0.984615384615383,1.),.UNSPECIFIED.)
CURVE()
GEOMETRIC_REPRESENTATION_ITEM()
RATIONAL_B_SPLINE_CURVE((1.,1.,1.,1.,1.,1.,1.,1.,1.,1.,1.,1.,1.,1.,1.,1.,
1.,1.,1.,1.,1.,1.,1.,1.,1.,1.,1.,1.,1.,1.,1.,1.,1.,1.,1.,1.,1.,1.,1.,1.,
1.,1.,1.,1.,1.,1.,1.,1.,1.,1.,1.,1.,1.,1.,1.,1.,1.,1.,1.,1.,1.,1.,1.,1.,
1.,1.,1.,1.,1.,1.))
REPRESENTATION_ITEM('')
);
#54=(
BOUNDED_CURVE()
B_SPLINE_CURVE(5,(#21608,#21609,#21610,#21611,#21612,#21613,#21614,#21615,
#21616,#21617,#21618,#21619,#21620,#21621,#21622,#21623,#21624,#21625,#21626,
#21627,#21628,#21629,#21630,#21631,#21632,#21633,#21634,#21635,#21636,#21637,
#21638,#21639,#21640,#21641,#21642,#21643,#21644,#21645,#21646,#21647,#21648,
#21649,#21650,#21651,#21652,#21653,#21654,#21655,#21656,#21657,#21658,#21659,
#21660,#21661,#21662,#21663,#21664,#21665,#21666,#21667,#21668,#21669,#21670,
#21671,#21672,#21673,#21674,#21675,#21676,#21677),.UNSPECIFIED.,.F.,.F.)
B_SPLINE_CURVE_WITH_KNOTS((6,1,1,1,1,1,1,1,1,1,1,1,1,1,1,1,1,1,1,1,1,1,
1,1,1,1,1,1,1,1,1,1,1,1,1,1,1,1,1,1,1,1,1,1,1,1,1,1,1,1,1,1,1,1,1,1,1,1,
1,1,1,1,1,1,1,6),(0.,0.0153846153846154,0.0307692307692308,0.0461538461538462,
0.0615384615384615,0.0769230769230769,0.0923076923076923,0.107692307692308,
0.123076923076923,0.138461538461538,0.153846153846154,0.169230769230769,
0.184615384615385,0.2,0.215384615384615,0.230769230769231,0.246153846153846,
0.261538461538462,0.276923076923077,0.292307692307692,0.307692307692308,
0.323076923076923,0.338461538461538,0.353846153846154,0.369230769230769,
0.384615384615385,0.4,0.415384615384615,0.430769230769231,0.446153846153846,
0.461538461538462,0.476923076923077,0.492307692307692,0.507692307692308,
0.523076923076923,0.538461538461538,0.553846153846154,0.569230769230769,
0.584615384615384,0.6,0.615384615384615,0.63076923076923,0.646153846153846,
0.661538461538461,0.676923076923076,0.692307692307692,0.707692307692307,
0.723076923076922,0.738461538461538,0.753846153846153,0.769230769230768,
0.784615384615384,0.799999999999999,0.815384615384614,0.83076923076923,
0.846153846153845,0.86153846153846,0.876923076923076,0.892307692307691,
0.907692307692306,0.923076923076922,0.938461538461537,0.953846153846152,
0.969230769230768,0.984615384615383,1.),.UNSPECIFIED.)
CURVE()
GEOMETRIC_REPRESENTATION_ITEM()
RATIONAL_B_SPLINE_CURVE((1.,1.,1.,1.,1.,1.,1.,1.,1.,1.,1.,1.,1.,1.,1.,1.,
1.,1.,1.,1.,1.,1.,1.,1.,1.,1.,1.,1.,1.,1.,1.,1.,1.,1.,1.,1.,1.,1.,1.,1.,
1.,1.,1.,1.,1.,1.,1.,1.,1.,1.,1.,1.,1.,1.,1.,1.,1.,1.,1.,1.,1.,1.,1.,1.,
1.,1.,1.,1.,1.,1.))
REPRESENTATION_ITEM('')
);
#55=(
BOUNDED_CURVE()
B_SPLINE_CURVE(5,(#21681,#21682,#21683,#21684,#21685,#21686,#21687,#21688,
#21689,#21690,#21691,#21692,#21693,#21694,#21695,#21696,#21697,#21698,#21699,
#21700,#21701,#21702,#21703,#21704,#21705,#21706,#21707,#21708,#21709,#21710,
#21711,#21712,#21713,#21714,#21715,#21716,#21717,#21718,#21719,#21720,#21721,
#21722,#21723,#21724,#21725,#21726,#21727,#21728,#21729,#21730,#21731,#21732,
#21733,#21734,#21735,#21736,#21737,#21738,#21739,#21740,#21741,#21742,#21743,
#21744,#21745,#21746,#21747,#21748,#21749,#21750),.UNSPECIFIED.,.F.,.F.)
B_SPLINE_CURVE_WITH_KNOTS((6,1,1,1,1,1,1,1,1,1,1,1,1,1,1,1,1,1,1,1,1,1,
1,1,1,1,1,1,1,1,1,1,1,1,1,1,1,1,1,1,1,1,1,1,1,1,1,1,1,1,1,1,1,1,1,1,1,1,
1,1,1,1,1,1,1,6),(0.,0.0153846153846154,0.0307692307692308,0.0461538461538462,
0.0615384615384615,0.0769230769230769,0.0923076923076923,0.107692307692308,
0.123076923076923,0.138461538461538,0.153846153846154,0.169230769230769,
0.184615384615385,0.2,0.215384615384615,0.230769230769231,0.246153846153846,
0.261538461538462,0.276923076923077,0.292307692307692,0.307692307692308,
0.323076923076923,0.338461538461538,0.353846153846154,0.369230769230769,
0.384615384615385,0.4,0.415384615384615,0.430769230769231,0.446153846153846,
0.461538461538462,0.476923076923077,0.492307692307692,0.507692307692308,
0.523076923076923,0.538461538461538,0.553846153846154,0.569230769230769,
0.584615384615384,0.6,0.615384615384615,0.63076923076923,0.646153846153846,
0.661538461538461,0.676923076923076,0.692307692307692,0.707692307692307,
0.723076923076922,0.738461538461538,0.753846153846153,0.769230769230768,
0.784615384615384,0.799999999999999,0.815384615384614,0.83076923076923,
0.846153846153845,0.86153846153846,0.876923076923076,0.892307692307691,
0.907692307692306,0.923076923076922,0.938461538461537,0.953846153846152,
0.969230769230768,0.984615384615383,1.),.UNSPECIFIED.)
CURVE()
GEOMETRIC_REPRESENTATION_ITEM()
RATIONAL_B_SPLINE_CURVE((1.,1.,1.,1.,1.,1.,1.,1.,1.,1.,1.,1.,1.,1.,1.,1.,
1.,1.,1.,1.,1.,1.,1.,1.,1.,1.,1.,1.,1.,1.,1.,1.,1.,1.,1.,1.,1.,1.,1.,1.,
1.,1.,1.,1.,1.,1.,1.,1.,1.,1.,1.,1.,1.,1.,1.,1.,1.,1.,1.,1.,1.,1.,1.,1.,
1.,1.,1.,1.,1.,1.))
REPRESENTATION_ITEM('')
);
#56=(
BOUNDED_CURVE()
B_SPLINE_CURVE(5,(#21754,#21755,#21756,#21757,#21758,#21759,#21760,#21761,
#21762,#21763,#21764,#21765,#21766,#21767,#21768,#21769,#21770,#21771,#21772,
#21773,#21774,#21775,#21776,#21777,#21778,#21779,#21780,#21781,#21782,#21783,
#21784,#21785,#21786,#21787,#21788,#21789,#21790,#21791,#21792,#21793,#21794,
#21795,#21796,#21797,#21798,#21799,#21800,#21801,#21802,#21803,#21804,#21805,
#21806,#21807,#21808,#21809,#21810,#21811,#21812,#21813,#21814,#21815,#21816,
#21817,#21818,#21819,#21820,#21821,#21822,#21823),.UNSPECIFIED.,.F.,.F.)
B_SPLINE_CURVE_WITH_KNOTS((6,1,1,1,1,1,1,1,1,1,1,1,1,1,1,1,1,1,1,1,1,1,
1,1,1,1,1,1,1,1,1,1,1,1,1,1,1,1,1,1,1,1,1,1,1,1,1,1,1,1,1,1,1,1,1,1,1,1,
1,1,1,1,1,1,1,6),(0.,0.0153846153846154,0.0307692307692308,0.0461538461538462,
0.0615384615384615,0.0769230769230769,0.0923076923076923,0.107692307692308,
0.123076923076923,0.138461538461538,0.153846153846154,0.169230769230769,
0.184615384615385,0.2,0.215384615384615,0.230769230769231,0.246153846153846,
0.261538461538462,0.276923076923077,0.292307692307692,0.307692307692308,
0.323076923076923,0.338461538461538,0.353846153846154,0.369230769230769,
0.384615384615385,0.4,0.415384615384615,0.430769230769231,0.446153846153846,
0.461538461538462,0.476923076923077,0.492307692307692,0.507692307692308,
0.523076923076923,0.538461538461538,0.553846153846154,0.569230769230769,
0.584615384615384,0.6,0.615384615384615,0.63076923076923,0.646153846153846,
0.661538461538461,0.676923076923076,0.692307692307692,0.707692307692307,
0.723076923076922,0.738461538461538,0.753846153846153,0.769230769230768,
0.784615384615384,0.799999999999999,0.815384615384614,0.83076923076923,
0.846153846153845,0.86153846153846,0.876923076923076,0.892307692307691,
0.907692307692306,0.923076923076922,0.938461538461537,0.953846153846152,
0.969230769230768,0.984615384615383,1.),.UNSPECIFIED.)
CURVE()
GEOMETRIC_REPRESENTATION_ITEM()
RATIONAL_B_SPLINE_CURVE((1.,1.,1.,1.,1.,1.,1.,1.,1.,1.,1.,1.,1.,1.,1.,1.,
1.,1.,1.,1.,1.,1.,1.,1.,1.,1.,1.,1.,1.,1.,1.,1.,1.,1.,1.,1.,1.,1.,1.,1.,
1.,1.,1.,1.,1.,1.,1.,1.,1.,1.,1.,1.,1.,1.,1.,1.,1.,1.,1.,1.,1.,1.,1.,1.,
1.,1.,1.,1.,1.,1.))
REPRESENTATION_ITEM('')
);
#57=(
BOUNDED_CURVE()
B_SPLINE_CURVE(5,(#21827,#21828,#21829,#21830,#21831,#21832,#21833,#21834,
#21835,#21836,#21837,#21838,#21839,#21840,#21841,#21842,#21843,#21844,#21845,
#21846,#21847,#21848,#21849,#21850,#21851,#21852,#21853,#21854,#21855,#21856,
#21857,#21858,#21859,#21860,#21861,#21862,#21863,#21864,#21865,#21866,#21867,
#21868,#21869,#21870,#21871,#21872,#21873,#21874,#21875,#21876,#21877,#21878,
#21879,#21880,#21881,#21882,#21883,#21884,#21885,#21886,#21887,#21888,#21889,
#21890,#21891,#21892,#21893,#21894,#21895,#21896),.UNSPECIFIED.,.F.,.F.)
B_SPLINE_CURVE_WITH_KNOTS((6,1,1,1,1,1,1,1,1,1,1,1,1,1,1,1,1,1,1,1,1,1,
1,1,1,1,1,1,1,1,1,1,1,1,1,1,1,1,1,1,1,1,1,1,1,1,1,1,1,1,1,1,1,1,1,1,1,1,
1,1,1,1,1,1,1,6),(0.,0.0153846153846154,0.0307692307692308,0.0461538461538462,
0.0615384615384615,0.0769230769230769,0.0923076923076923,0.107692307692308,
0.123076923076923,0.138461538461538,0.153846153846154,0.169230769230769,
0.184615384615385,0.2,0.215384615384615,0.230769230769231,0.246153846153846,
0.261538461538462,0.276923076923077,0.292307692307692,0.307692307692308,
0.323076923076923,0.338461538461538,0.353846153846154,0.369230769230769,
0.384615384615385,0.4,0.415384615384615,0.430769230769231,0.446153846153846,
0.461538461538462,0.476923076923077,0.492307692307692,0.507692307692308,
0.523076923076923,0.538461538461538,0.553846153846154,0.569230769230769,
0.584615384615384,0.6,0.615384615384615,0.63076923076923,0.646153846153846,
0.661538461538461,0.676923076923076,0.692307692307692,0.707692307692307,
0.723076923076922,0.738461538461538,0.753846153846153,0.769230769230768,
0.784615384615384,0.799999999999999,0.815384615384614,0.83076923076923,
0.846153846153845,0.86153846153846,0.876923076923076,0.892307692307691,
0.907692307692306,0.923076923076922,0.938461538461537,0.953846153846152,
0.969230769230768,0.984615384615383,1.),.UNSPECIFIED.)
CURVE()
GEOMETRIC_REPRESENTATION_ITEM()
RATIONAL_B_SPLINE_CURVE((1.,1.,1.,1.,1.,1.,1.,1.,1.,1.,1.,1.,1.,1.,1.,1.,
1.,1.,1.,1.,1.,1.,1.,1.,1.,1.,1.,1.,1.,1.,1.,1.,1.,1.,1.,1.,1.,1.,1.,1.,
1.,1.,1.,1.,1.,1.,1.,1.,1.,1.,1.,1.,1.,1.,1.,1.,1.,1.,1.,1.,1.,1.,1.,1.,
1.,1.,1.,1.,1.,1.))
REPRESENTATION_ITEM('')
);
#58=(
BOUNDED_CURVE()
B_SPLINE_CURVE(5,(#21900,#21901,#21902,#21903,#21904,#21905,#21906,#21907,
#21908,#21909,#21910,#21911,#21912,#21913,#21914,#21915,#21916,#21917,#21918,
#21919,#21920,#21921,#21922,#21923,#21924,#21925,#21926,#21927,#21928,#21929,
#21930,#21931,#21932,#21933,#21934,#21935,#21936,#21937,#21938,#21939,#21940,
#21941,#21942,#21943,#21944,#21945,#21946,#21947,#21948,#21949,#21950,#21951,
#21952,#21953,#21954,#21955,#21956,#21957,#21958,#21959,#21960,#21961,#21962,
#21963,#21964,#21965,#21966,#21967,#21968,#21969),.UNSPECIFIED.,.F.,.F.)
B_SPLINE_CURVE_WITH_KNOTS((6,1,1,1,1,1,1,1,1,1,1,1,1,1,1,1,1,1,1,1,1,1,
1,1,1,1,1,1,1,1,1,1,1,1,1,1,1,1,1,1,1,1,1,1,1,1,1,1,1,1,1,1,1,1,1,1,1,1,
1,1,1,1,1,1,1,6),(0.,0.0153846153846154,0.0307692307692308,0.0461538461538462,
0.0615384615384615,0.0769230769230769,0.0923076923076923,0.107692307692308,
0.123076923076923,0.138461538461538,0.153846153846154,0.169230769230769,
0.184615384615385,0.2,0.215384615384615,0.230769230769231,0.246153846153846,
0.261538461538462,0.276923076923077,0.292307692307692,0.307692307692308,
0.323076923076923,0.338461538461538,0.353846153846154,0.369230769230769,
0.384615384615385,0.4,0.415384615384615,0.430769230769231,0.446153846153846,
0.461538461538462,0.476923076923077,0.492307692307692,0.507692307692308,
0.523076923076923,0.538461538461538,0.553846153846154,0.569230769230769,
0.584615384615384,0.6,0.615384615384615,0.63076923076923,0.646153846153846,
0.661538461538461,0.676923076923076,0.692307692307692,0.707692307692307,
0.723076923076922,0.738461538461538,0.753846153846153,0.769230769230768,
0.784615384615384,0.799999999999999,0.815384615384614,0.83076923076923,
0.846153846153845,0.86153846153846,0.876923076923076,0.892307692307691,
0.907692307692306,0.923076923076922,0.938461538461537,0.953846153846152,
0.969230769230768,0.984615384615383,1.),.UNSPECIFIED.)
CURVE()
GEOMETRIC_REPRESENTATION_ITEM()
RATIONAL_B_SPLINE_CURVE((1.,1.,1.,1.,1.,1.,1.,1.,1.,1.,1.,1.,1.,1.,1.,1.,
1.,1.,1.,1.,1.,1.,1.,1.,1.,1.,1.,1.,1.,1.,1.,1.,1.,1.,1.,1.,1.,1.,1.,1.,
1.,1.,1.,1.,1.,1.,1.,1.,1.,1.,1.,1.,1.,1.,1.,1.,1.,1.,1.,1.,1.,1.,1.,1.,
1.,1.,1.,1.,1.,1.))
REPRESENTATION_ITEM('')
);
#59=(
BOUNDED_CURVE()
B_SPLINE_CURVE(5,(#21973,#21974,#21975,#21976,#21977,#21978,#21979,#21980,
#21981,#21982,#21983,#21984,#21985,#21986,#21987,#21988,#21989,#21990,#21991,
#21992,#21993,#21994,#21995,#21996,#21997,#21998,#21999,#22000,#22001,#22002,
#22003,#22004,#22005,#22006,#22007,#22008,#22009,#22010,#22011,#22012,#22013,
#22014,#22015,#22016,#22017,#22018,#22019,#22020,#22021,#22022,#22023,#22024,
#22025,#22026,#22027,#22028,#22029,#22030,#22031,#22032,#22033,#22034,#22035,
#22036,#22037,#22038,#22039,#22040,#22041,#22042),.UNSPECIFIED.,.F.,.F.)
B_SPLINE_CURVE_WITH_KNOTS((6,1,1,1,1,1,1,1,1,1,1,1,1,1,1,1,1,1,1,1,1,1,
1,1,1,1,1,1,1,1,1,1,1,1,1,1,1,1,1,1,1,1,1,1,1,1,1,1,1,1,1,1,1,1,1,1,1,1,
1,1,1,1,1,1,1,6),(0.,0.0153846153846154,0.0307692307692308,0.0461538461538462,
0.0615384615384615,0.0769230769230769,0.0923076923076923,0.107692307692308,
0.123076923076923,0.138461538461538,0.153846153846154,0.169230769230769,
0.184615384615385,0.2,0.215384615384615,0.230769230769231,0.246153846153846,
0.261538461538462,0.276923076923077,0.292307692307692,0.307692307692308,
0.323076923076923,0.338461538461538,0.353846153846154,0.369230769230769,
0.384615384615385,0.4,0.415384615384615,0.430769230769231,0.446153846153846,
0.461538461538462,0.476923076923077,0.492307692307692,0.507692307692308,
0.523076923076923,0.538461538461538,0.553846153846154,0.569230769230769,
0.584615384615384,0.6,0.615384615384615,0.63076923076923,0.646153846153846,
0.661538461538461,0.676923076923076,0.692307692307692,0.707692307692307,
0.723076923076922,0.738461538461538,0.753846153846153,0.769230769230768,
0.784615384615384,0.799999999999999,0.815384615384614,0.83076923076923,
0.846153846153845,0.86153846153846,0.876923076923076,0.892307692307691,
0.907692307692306,0.923076923076922,0.938461538461537,0.953846153846152,
0.969230769230768,0.984615384615383,1.),.UNSPECIFIED.)
CURVE()
GEOMETRIC_REPRESENTATION_ITEM()
RATIONAL_B_SPLINE_CURVE((1.,1.,1.,1.,1.,1.,1.,1.,1.,1.,1.,1.,1.,1.,1.,1.,
1.,1.,1.,1.,1.,1.,1.,1.,1.,1.,1.,1.,1.,1.,1.,1.,1.,1.,1.,1.,1.,1.,1.,1.,
1.,1.,1.,1.,1.,1.,1.,1.,1.,1.,1.,1.,1.,1.,1.,1.,1.,1.,1.,1.,1.,1.,1.,1.,
1.,1.,1.,1.,1.,1.))
REPRESENTATION_ITEM('')
);
#60=(
BOUNDED_CURVE()
B_SPLINE_CURVE(5,(#22046,#22047,#22048,#22049,#22050,#22051,#22052,#22053,
#22054,#22055,#22056,#22057,#22058,#22059,#22060,#22061,#22062,#22063,#22064,
#22065,#22066,#22067,#22068,#22069,#22070,#22071,#22072,#22073,#22074,#22075,
#22076,#22077,#22078,#22079,#22080,#22081,#22082,#22083,#22084,#22085,#22086,
#22087,#22088,#22089,#22090,#22091,#22092,#22093,#22094,#22095,#22096,#22097,
#22098,#22099,#22100,#22101,#22102,#22103,#22104,#22105,#22106,#22107,#22108,
#22109,#22110,#22111,#22112,#22113,#22114,#22115),.UNSPECIFIED.,.F.,.F.)
B_SPLINE_CURVE_WITH_KNOTS((6,1,1,1,1,1,1,1,1,1,1,1,1,1,1,1,1,1,1,1,1,1,
1,1,1,1,1,1,1,1,1,1,1,1,1,1,1,1,1,1,1,1,1,1,1,1,1,1,1,1,1,1,1,1,1,1,1,1,
1,1,1,1,1,1,1,6),(0.,0.0153846153846154,0.0307692307692308,0.0461538461538462,
0.0615384615384615,0.0769230769230769,0.0923076923076923,0.107692307692308,
0.123076923076923,0.138461538461538,0.153846153846154,0.169230769230769,
0.184615384615385,0.2,0.215384615384615,0.230769230769231,0.246153846153846,
0.261538461538462,0.276923076923077,0.292307692307692,0.307692307692308,
0.323076923076923,0.338461538461538,0.353846153846154,0.369230769230769,
0.384615384615385,0.4,0.415384615384615,0.430769230769231,0.446153846153846,
0.461538461538462,0.476923076923077,0.492307692307692,0.507692307692308,
0.523076923076923,0.538461538461538,0.553846153846154,0.569230769230769,
0.584615384615384,0.6,0.615384615384615,0.63076923076923,0.646153846153846,
0.661538461538461,0.676923076923076,0.692307692307692,0.707692307692307,
0.723076923076922,0.738461538461538,0.753846153846153,0.769230769230768,
0.784615384615384,0.799999999999999,0.815384615384614,0.83076923076923,
0.846153846153845,0.86153846153846,0.876923076923076,0.892307692307691,
0.907692307692306,0.923076923076922,0.938461538461537,0.953846153846152,
0.969230769230768,0.984615384615383,1.),.UNSPECIFIED.)
CURVE()
GEOMETRIC_REPRESENTATION_ITEM()
RATIONAL_B_SPLINE_CURVE((1.,1.,1.,1.,1.,1.,1.,1.,1.,1.,1.,1.,1.,1.,1.,1.,
1.,1.,1.,1.,1.,1.,1.,1.,1.,1.,1.,1.,1.,1.,1.,1.,1.,1.,1.,1.,1.,1.,1.,1.,
1.,1.,1.,1.,1.,1.,1.,1.,1.,1.,1.,1.,1.,1.,1.,1.,1.,1.,1.,1.,1.,1.,1.,1.,
1.,1.,1.,1.,1.,1.))
REPRESENTATION_ITEM('')
);
#61=(
BOUNDED_CURVE()
B_SPLINE_CURVE(5,(#22119,#22120,#22121,#22122,#22123,#22124,#22125,#22126,
#22127,#22128,#22129,#22130,#22131,#22132,#22133,#22134,#22135,#22136,#22137,
#22138,#22139,#22140,#22141,#22142,#22143,#22144,#22145,#22146,#22147,#22148,
#22149,#22150,#22151,#22152,#22153,#22154,#22155,#22156,#22157,#22158,#22159,
#22160,#22161,#22162,#22163,#22164,#22165,#22166,#22167,#22168,#22169,#22170,
#22171,#22172,#22173,#22174,#22175,#22176,#22177,#22178,#22179,#22180,#22181,
#22182,#22183,#22184,#22185,#22186,#22187,#22188),.UNSPECIFIED.,.F.,.F.)
B_SPLINE_CURVE_WITH_KNOTS((6,1,1,1,1,1,1,1,1,1,1,1,1,1,1,1,1,1,1,1,1,1,
1,1,1,1,1,1,1,1,1,1,1,1,1,1,1,1,1,1,1,1,1,1,1,1,1,1,1,1,1,1,1,1,1,1,1,1,
1,1,1,1,1,1,1,6),(0.,0.0153846153846154,0.0307692307692308,0.0461538461538462,
0.0615384615384615,0.0769230769230769,0.0923076923076923,0.107692307692308,
0.123076923076923,0.138461538461538,0.153846153846154,0.169230769230769,
0.184615384615385,0.2,0.215384615384615,0.230769230769231,0.246153846153846,
0.261538461538462,0.276923076923077,0.292307692307692,0.307692307692308,
0.323076923076923,0.338461538461538,0.353846153846154,0.369230769230769,
0.384615384615385,0.4,0.415384615384615,0.430769230769231,0.446153846153846,
0.461538461538462,0.476923076923077,0.492307692307692,0.507692307692308,
0.523076923076923,0.538461538461538,0.553846153846154,0.569230769230769,
0.584615384615384,0.6,0.615384615384615,0.63076923076923,0.646153846153846,
0.661538461538461,0.676923076923076,0.692307692307692,0.707692307692307,
0.723076923076922,0.738461538461538,0.753846153846153,0.769230769230768,
0.784615384615384,0.799999999999999,0.815384615384614,0.83076923076923,
0.846153846153845,0.86153846153846,0.876923076923076,0.892307692307691,
0.907692307692306,0.923076923076922,0.938461538461537,0.953846153846152,
0.969230769230768,0.984615384615383,1.),.UNSPECIFIED.)
CURVE()
GEOMETRIC_REPRESENTATION_ITEM()
RATIONAL_B_SPLINE_CURVE((1.,1.,1.,1.,1.,1.,1.,1.,1.,1.,1.,1.,1.,1.,1.,1.,
1.,1.,1.,1.,1.,1.,1.,1.,1.,1.,1.,1.,1.,1.,1.,1.,1.,1.,1.,1.,1.,1.,1.,1.,
1.,1.,1.,1.,1.,1.,1.,1.,1.,1.,1.,1.,1.,1.,1.,1.,1.,1.,1.,1.,1.,1.,1.,1.,
1.,1.,1.,1.,1.,1.))
REPRESENTATION_ITEM('')
);
#62=(
BOUNDED_CURVE()
B_SPLINE_CURVE(5,(#22192,#22193,#22194,#22195,#22196,#22197,#22198,#22199,
#22200,#22201,#22202,#22203,#22204,#22205,#22206,#22207,#22208,#22209,#22210,
#22211,#22212,#22213,#22214,#22215,#22216,#22217,#22218,#22219,#22220,#22221,
#22222,#22223,#22224,#22225,#22226,#22227,#22228,#22229,#22230,#22231,#22232,
#22233,#22234,#22235,#22236,#22237,#22238,#22239,#22240,#22241,#22242,#22243,
#22244,#22245,#22246,#22247,#22248,#22249,#22250,#22251,#22252,#22253,#22254,
#22255,#22256,#22257,#22258,#22259,#22260,#22261),.UNSPECIFIED.,.F.,.F.)
B_SPLINE_CURVE_WITH_KNOTS((6,1,1,1,1,1,1,1,1,1,1,1,1,1,1,1,1,1,1,1,1,1,
1,1,1,1,1,1,1,1,1,1,1,1,1,1,1,1,1,1,1,1,1,1,1,1,1,1,1,1,1,1,1,1,1,1,1,1,
1,1,1,1,1,1,1,6),(0.,0.0153846153846154,0.0307692307692308,0.0461538461538462,
0.0615384615384615,0.0769230769230769,0.0923076923076923,0.107692307692308,
0.123076923076923,0.138461538461538,0.153846153846154,0.169230769230769,
0.184615384615385,0.2,0.215384615384615,0.230769230769231,0.246153846153846,
0.261538461538462,0.276923076923077,0.292307692307692,0.307692307692308,
0.323076923076923,0.338461538461538,0.353846153846154,0.369230769230769,
0.384615384615385,0.4,0.415384615384615,0.430769230769231,0.446153846153846,
0.461538461538462,0.476923076923077,0.492307692307692,0.507692307692308,
0.523076923076923,0.538461538461538,0.553846153846154,0.569230769230769,
0.584615384615384,0.6,0.615384615384615,0.63076923076923,0.646153846153846,
0.661538461538461,0.676923076923076,0.692307692307692,0.707692307692307,
0.723076923076922,0.738461538461538,0.753846153846153,0.769230769230768,
0.784615384615384,0.799999999999999,0.815384615384614,0.83076923076923,
0.846153846153845,0.86153846153846,0.876923076923076,0.892307692307691,
0.907692307692306,0.923076923076922,0.938461538461537,0.953846153846152,
0.969230769230768,0.984615384615383,1.),.UNSPECIFIED.)
CURVE()
GEOMETRIC_REPRESENTATION_ITEM()
RATIONAL_B_SPLINE_CURVE((1.,1.,1.,1.,1.,1.,1.,1.,1.,1.,1.,1.,1.,1.,1.,1.,
1.,1.,1.,1.,1.,1.,1.,1.,1.,1.,1.,1.,1.,1.,1.,1.,1.,1.,1.,1.,1.,1.,1.,1.,
1.,1.,1.,1.,1.,1.,1.,1.,1.,1.,1.,1.,1.,1.,1.,1.,1.,1.,1.,1.,1.,1.,1.,1.,
1.,1.,1.,1.,1.,1.))
REPRESENTATION_ITEM('')
);
#63=(
BOUNDED_CURVE()
B_SPLINE_CURVE(5,(#22265,#22266,#22267,#22268,#22269,#22270,#22271,#22272,
#22273,#22274,#22275,#22276,#22277,#22278,#22279,#22280,#22281,#22282,#22283,
#22284,#22285,#22286,#22287,#22288,#22289,#22290,#22291,#22292,#22293,#22294,
#22295,#22296,#22297,#22298,#22299,#22300,#22301,#22302,#22303,#22304,#22305,
#22306,#22307,#22308,#22309,#22310,#22311,#22312,#22313,#22314,#22315,#22316,
#22317,#22318,#22319,#22320,#22321,#22322,#22323,#22324,#22325,#22326,#22327,
#22328,#22329,#22330,#22331,#22332,#22333,#22334),.UNSPECIFIED.,.F.,.F.)
B_SPLINE_CURVE_WITH_KNOTS((6,1,1,1,1,1,1,1,1,1,1,1,1,1,1,1,1,1,1,1,1,1,
1,1,1,1,1,1,1,1,1,1,1,1,1,1,1,1,1,1,1,1,1,1,1,1,1,1,1,1,1,1,1,1,1,1,1,1,
1,1,1,1,1,1,1,6),(0.,0.0153846153846154,0.0307692307692308,0.0461538461538462,
0.0615384615384615,0.0769230769230769,0.0923076923076923,0.107692307692308,
0.123076923076923,0.138461538461538,0.153846153846154,0.169230769230769,
0.184615384615385,0.2,0.215384615384615,0.230769230769231,0.246153846153846,
0.261538461538462,0.276923076923077,0.292307692307692,0.307692307692308,
0.323076923076923,0.338461538461538,0.353846153846154,0.369230769230769,
0.384615384615385,0.4,0.415384615384615,0.430769230769231,0.446153846153846,
0.461538461538462,0.476923076923077,0.492307692307692,0.507692307692308,
0.523076923076923,0.538461538461538,0.553846153846154,0.569230769230769,
0.584615384615384,0.6,0.615384615384615,0.63076923076923,0.646153846153846,
0.661538461538461,0.676923076923076,0.692307692307692,0.707692307692307,
0.723076923076922,0.738461538461538,0.753846153846153,0.769230769230768,
0.784615384615384,0.799999999999999,0.815384615384614,0.83076923076923,
0.846153846153845,0.86153846153846,0.876923076923076,0.892307692307691,
0.907692307692306,0.923076923076922,0.938461538461537,0.953846153846152,
0.969230769230768,0.984615384615383,1.),.UNSPECIFIED.)
CURVE()
GEOMETRIC_REPRESENTATION_ITEM()
RATIONAL_B_SPLINE_CURVE((1.,1.,1.,1.,1.,1.,1.,1.,1.,1.,1.,1.,1.,1.,1.,1.,
1.,1.,1.,1.,1.,1.,1.,1.,1.,1.,1.,1.,1.,1.,1.,1.,1.,1.,1.,1.,1.,1.,1.,1.,
1.,1.,1.,1.,1.,1.,1.,1.,1.,1.,1.,1.,1.,1.,1.,1.,1.,1.,1.,1.,1.,1.,1.,1.,
1.,1.,1.,1.,1.,1.))
REPRESENTATION_ITEM('')
);
#64=(
BOUNDED_CURVE()
B_SPLINE_CURVE(5,(#22338,#22339,#22340,#22341,#22342,#22343,#22344,#22345,
#22346,#22347,#22348,#22349,#22350,#22351,#22352,#22353,#22354,#22355,#22356,
#22357,#22358,#22359,#22360,#22361,#22362,#22363,#22364,#22365,#22366,#22367,
#22368,#22369,#22370,#22371,#22372,#22373,#22374,#22375,#22376,#22377,#22378,
#22379,#22380,#22381,#22382,#22383,#22384,#22385,#22386,#22387,#22388,#22389,
#22390,#22391,#22392,#22393,#22394,#22395,#22396,#22397,#22398,#22399,#22400,
#22401,#22402,#22403,#22404,#22405,#22406,#22407),.UNSPECIFIED.,.F.,.F.)
B_SPLINE_CURVE_WITH_KNOTS((6,1,1,1,1,1,1,1,1,1,1,1,1,1,1,1,1,1,1,1,1,1,
1,1,1,1,1,1,1,1,1,1,1,1,1,1,1,1,1,1,1,1,1,1,1,1,1,1,1,1,1,1,1,1,1,1,1,1,
1,1,1,1,1,1,1,6),(0.,0.0153846153846154,0.0307692307692308,0.0461538461538462,
0.0615384615384615,0.0769230769230769,0.0923076923076923,0.107692307692308,
0.123076923076923,0.138461538461538,0.153846153846154,0.169230769230769,
0.184615384615385,0.2,0.215384615384615,0.230769230769231,0.246153846153846,
0.261538461538462,0.276923076923077,0.292307692307692,0.307692307692308,
0.323076923076923,0.338461538461538,0.353846153846154,0.369230769230769,
0.384615384615385,0.4,0.415384615384615,0.430769230769231,0.446153846153846,
0.461538461538462,0.476923076923077,0.492307692307692,0.507692307692308,
0.523076923076923,0.538461538461538,0.553846153846154,0.569230769230769,
0.584615384615384,0.6,0.615384615384615,0.63076923076923,0.646153846153846,
0.661538461538461,0.676923076923076,0.692307692307692,0.707692307692307,
0.723076923076922,0.738461538461538,0.753846153846153,0.769230769230768,
0.784615384615384,0.799999999999999,0.815384615384614,0.83076923076923,
0.846153846153845,0.86153846153846,0.876923076923076,0.892307692307691,
0.907692307692306,0.923076923076922,0.938461538461537,0.953846153846152,
0.969230769230768,0.984615384615383,1.),.UNSPECIFIED.)
CURVE()
GEOMETRIC_REPRESENTATION_ITEM()
RATIONAL_B_SPLINE_CURVE((1.,1.,1.,1.,1.,1.,1.,1.,1.,1.,1.,1.,1.,1.,1.,1.,
1.,1.,1.,1.,1.,1.,1.,1.,1.,1.,1.,1.,1.,1.,1.,1.,1.,1.,1.,1.,1.,1.,1.,1.,
1.,1.,1.,1.,1.,1.,1.,1.,1.,1.,1.,1.,1.,1.,1.,1.,1.,1.,1.,1.,1.,1.,1.,1.,
1.,1.,1.,1.,1.,1.))
REPRESENTATION_ITEM('')
);
#65=(
BOUNDED_CURVE()
B_SPLINE_CURVE(5,(#22411,#22412,#22413,#22414,#22415,#22416,#22417,#22418,
#22419,#22420,#22421,#22422,#22423,#22424,#22425,#22426,#22427,#22428,#22429,
#22430,#22431,#22432,#22433,#22434,#22435,#22436,#22437,#22438,#22439,#22440,
#22441,#22442,#22443,#22444,#22445,#22446,#22447,#22448,#22449,#22450,#22451,
#22452,#22453,#22454,#22455,#22456,#22457,#22458,#22459,#22460,#22461,#22462,
#22463,#22464,#22465,#22466,#22467,#22468,#22469,#22470,#22471,#22472,#22473,
#22474,#22475,#22476,#22477,#22478,#22479,#22480),.UNSPECIFIED.,.F.,.F.)
B_SPLINE_CURVE_WITH_KNOTS((6,1,1,1,1,1,1,1,1,1,1,1,1,1,1,1,1,1,1,1,1,1,
1,1,1,1,1,1,1,1,1,1,1,1,1,1,1,1,1,1,1,1,1,1,1,1,1,1,1,1,1,1,1,1,1,1,1,1,
1,1,1,1,1,1,1,6),(0.,0.0153846153846154,0.0307692307692308,0.0461538461538462,
0.0615384615384615,0.0769230769230769,0.0923076923076923,0.107692307692308,
0.123076923076923,0.138461538461538,0.153846153846154,0.169230769230769,
0.184615384615385,0.2,0.215384615384615,0.230769230769231,0.246153846153846,
0.261538461538462,0.276923076923077,0.292307692307692,0.307692307692308,
0.323076923076923,0.338461538461538,0.353846153846154,0.369230769230769,
0.384615384615385,0.4,0.415384615384615,0.430769230769231,0.446153846153846,
0.461538461538462,0.476923076923077,0.492307692307692,0.507692307692308,
0.523076923076923,0.538461538461538,0.553846153846154,0.569230769230769,
0.584615384615384,0.6,0.615384615384615,0.63076923076923,0.646153846153846,
0.661538461538461,0.676923076923076,0.692307692307692,0.707692307692307,
0.723076923076922,0.738461538461538,0.753846153846153,0.769230769230768,
0.784615384615384,0.799999999999999,0.815384615384614,0.83076923076923,
0.846153846153845,0.86153846153846,0.876923076923076,0.892307692307691,
0.907692307692306,0.923076923076922,0.938461538461537,0.953846153846152,
0.969230769230768,0.984615384615383,1.),.UNSPECIFIED.)
CURVE()
GEOMETRIC_REPRESENTATION_ITEM()
RATIONAL_B_SPLINE_CURVE((1.,1.,1.,1.,1.,1.,1.,1.,1.,1.,1.,1.,1.,1.,1.,1.,
1.,1.,1.,1.,1.,1.,1.,1.,1.,1.,1.,1.,1.,1.,1.,1.,1.,1.,1.,1.,1.,1.,1.,1.,
1.,1.,1.,1.,1.,1.,1.,1.,1.,1.,1.,1.,1.,1.,1.,1.,1.,1.,1.,1.,1.,1.,1.,1.,
1.,1.,1.,1.,1.,1.))
REPRESENTATION_ITEM('')
);
#66=(
BOUNDED_CURVE()
B_SPLINE_CURVE(5,(#22484,#22485,#22486,#22487,#22488,#22489,#22490,#22491,
#22492,#22493,#22494,#22495,#22496,#22497,#22498,#22499,#22500,#22501,#22502,
#22503,#22504,#22505,#22506,#22507,#22508,#22509,#22510,#22511,#22512,#22513,
#22514,#22515,#22516,#22517,#22518,#22519,#22520,#22521,#22522,#22523,#22524,
#22525,#22526,#22527,#22528,#22529,#22530,#22531,#22532,#22533,#22534,#22535,
#22536,#22537,#22538,#22539,#22540,#22541,#22542,#22543,#22544,#22545,#22546,
#22547,#22548,#22549,#22550,#22551,#22552,#22553),.UNSPECIFIED.,.F.,.F.)
B_SPLINE_CURVE_WITH_KNOTS((6,1,1,1,1,1,1,1,1,1,1,1,1,1,1,1,1,1,1,1,1,1,
1,1,1,1,1,1,1,1,1,1,1,1,1,1,1,1,1,1,1,1,1,1,1,1,1,1,1,1,1,1,1,1,1,1,1,1,
1,1,1,1,1,1,1,6),(0.,0.0153846153846154,0.0307692307692308,0.0461538461538462,
0.0615384615384615,0.0769230769230769,0.0923076923076923,0.107692307692308,
0.123076923076923,0.138461538461538,0.153846153846154,0.169230769230769,
0.184615384615385,0.2,0.215384615384615,0.230769230769231,0.246153846153846,
0.261538461538462,0.276923076923077,0.292307692307692,0.307692307692308,
0.323076923076923,0.338461538461538,0.353846153846154,0.369230769230769,
0.384615384615385,0.4,0.415384615384615,0.430769230769231,0.446153846153846,
0.461538461538462,0.476923076923077,0.492307692307692,0.507692307692308,
0.523076923076923,0.538461538461538,0.553846153846154,0.569230769230769,
0.584615384615384,0.6,0.615384615384615,0.63076923076923,0.646153846153846,
0.661538461538461,0.676923076923076,0.692307692307692,0.707692307692307,
0.723076923076922,0.738461538461538,0.753846153846153,0.769230769230768,
0.784615384615384,0.799999999999999,0.815384615384614,0.83076923076923,
0.846153846153845,0.86153846153846,0.876923076923076,0.892307692307691,
0.907692307692306,0.923076923076922,0.938461538461537,0.953846153846152,
0.969230769230768,0.984615384615383,1.),.UNSPECIFIED.)
CURVE()
GEOMETRIC_REPRESENTATION_ITEM()
RATIONAL_B_SPLINE_CURVE((1.,1.,1.,1.,1.,1.,1.,1.,1.,1.,1.,1.,1.,1.,1.,1.,
1.,1.,1.,1.,1.,1.,1.,1.,1.,1.,1.,1.,1.,1.,1.,1.,1.,1.,1.,1.,1.,1.,1.,1.,
1.,1.,1.,1.,1.,1.,1.,1.,1.,1.,1.,1.,1.,1.,1.,1.,1.,1.,1.,1.,1.,1.,1.,1.,
1.,1.,1.,1.,1.,1.))
REPRESENTATION_ITEM('')
);
#67=(
BOUNDED_CURVE()
B_SPLINE_CURVE(5,(#22557,#22558,#22559,#22560,#22561,#22562,#22563,#22564,
#22565,#22566,#22567,#22568,#22569,#22570,#22571,#22572,#22573,#22574,#22575,
#22576,#22577,#22578,#22579,#22580,#22581,#22582,#22583,#22584,#22585,#22586,
#22587,#22588,#22589,#22590,#22591,#22592,#22593,#22594,#22595,#22596,#22597,
#22598,#22599,#22600,#22601,#22602,#22603,#22604,#22605,#22606,#22607,#22608,
#22609,#22610,#22611,#22612,#22613,#22614,#22615,#22616,#22617,#22618,#22619,
#22620,#22621,#22622,#22623,#22624,#22625,#22626),.UNSPECIFIED.,.F.,.F.)
B_SPLINE_CURVE_WITH_KNOTS((6,1,1,1,1,1,1,1,1,1,1,1,1,1,1,1,1,1,1,1,1,1,
1,1,1,1,1,1,1,1,1,1,1,1,1,1,1,1,1,1,1,1,1,1,1,1,1,1,1,1,1,1,1,1,1,1,1,1,
1,1,1,1,1,1,1,6),(0.,0.0153846153846154,0.0307692307692308,0.0461538461538462,
0.0615384615384615,0.0769230769230769,0.0923076923076923,0.107692307692308,
0.123076923076923,0.138461538461538,0.153846153846154,0.169230769230769,
0.184615384615385,0.2,0.215384615384615,0.230769230769231,0.246153846153846,
0.261538461538462,0.276923076923077,0.292307692307692,0.307692307692308,
0.323076923076923,0.338461538461538,0.353846153846154,0.369230769230769,
0.384615384615385,0.4,0.415384615384615,0.430769230769231,0.446153846153846,
0.461538461538462,0.476923076923077,0.492307692307692,0.507692307692308,
0.523076923076923,0.538461538461538,0.553846153846154,0.569230769230769,
0.584615384615384,0.6,0.615384615384615,0.63076923076923,0.646153846153846,
0.661538461538461,0.676923076923076,0.692307692307692,0.707692307692307,
0.723076923076922,0.738461538461538,0.753846153846153,0.769230769230768,
0.784615384615384,0.799999999999999,0.815384615384614,0.83076923076923,
0.846153846153845,0.86153846153846,0.876923076923076,0.892307692307691,
0.907692307692306,0.923076923076922,0.938461538461537,0.953846153846152,
0.969230769230768,0.984615384615383,1.),.UNSPECIFIED.)
CURVE()
GEOMETRIC_REPRESENTATION_ITEM()
RATIONAL_B_SPLINE_CURVE((1.,1.,1.,1.,1.,1.,1.,1.,1.,1.,1.,1.,1.,1.,1.,1.,
1.,1.,1.,1.,1.,1.,1.,1.,1.,1.,1.,1.,1.,1.,1.,1.,1.,1.,1.,1.,1.,1.,1.,1.,
1.,1.,1.,1.,1.,1.,1.,1.,1.,1.,1.,1.,1.,1.,1.,1.,1.,1.,1.,1.,1.,1.,1.,1.,
1.,1.,1.,1.,1.,1.))
REPRESENTATION_ITEM('')
);
#68=(
BOUNDED_CURVE()
B_SPLINE_CURVE(5,(#22630,#22631,#22632,#22633,#22634,#22635,#22636,#22637,
#22638,#22639,#22640,#22641,#22642,#22643,#22644,#22645,#22646,#22647,#22648,
#22649,#22650,#22651,#22652,#22653,#22654,#22655,#22656,#22657,#22658,#22659,
#22660,#22661,#22662,#22663,#22664,#22665,#22666,#22667,#22668,#22669,#22670,
#22671,#22672,#22673,#22674,#22675,#22676,#22677,#22678,#22679,#22680,#22681,
#22682,#22683,#22684,#22685,#22686,#22687,#22688,#22689,#22690,#22691,#22692,
#22693,#22694,#22695,#22696,#22697,#22698,#22699),.UNSPECIFIED.,.F.,.F.)
B_SPLINE_CURVE_WITH_KNOTS((6,1,1,1,1,1,1,1,1,1,1,1,1,1,1,1,1,1,1,1,1,1,
1,1,1,1,1,1,1,1,1,1,1,1,1,1,1,1,1,1,1,1,1,1,1,1,1,1,1,1,1,1,1,1,1,1,1,1,
1,1,1,1,1,1,1,6),(0.,0.0153846153846154,0.0307692307692308,0.0461538461538462,
0.0615384615384615,0.0769230769230769,0.0923076923076923,0.107692307692308,
0.123076923076923,0.138461538461538,0.153846153846154,0.169230769230769,
0.184615384615385,0.2,0.215384615384615,0.230769230769231,0.246153846153846,
0.261538461538462,0.276923076923077,0.292307692307692,0.307692307692308,
0.323076923076923,0.338461538461538,0.353846153846154,0.369230769230769,
0.384615384615385,0.4,0.415384615384615,0.430769230769231,0.446153846153846,
0.461538461538462,0.476923076923077,0.492307692307692,0.507692307692308,
0.523076923076923,0.538461538461538,0.553846153846154,0.569230769230769,
0.584615384615384,0.6,0.615384615384615,0.63076923076923,0.646153846153846,
0.661538461538461,0.676923076923076,0.692307692307692,0.707692307692307,
0.723076923076922,0.738461538461538,0.753846153846153,0.769230769230768,
0.784615384615384,0.799999999999999,0.815384615384614,0.83076923076923,
0.846153846153845,0.86153846153846,0.876923076923076,0.892307692307691,
0.907692307692306,0.923076923076922,0.938461538461537,0.953846153846152,
0.969230769230768,0.984615384615383,1.),.UNSPECIFIED.)
CURVE()
GEOMETRIC_REPRESENTATION_ITEM()
RATIONAL_B_SPLINE_CURVE((1.,1.,1.,1.,1.,1.,1.,1.,1.,1.,1.,1.,1.,1.,1.,1.,
1.,1.,1.,1.,1.,1.,1.,1.,1.,1.,1.,1.,1.,1.,1.,1.,1.,1.,1.,1.,1.,1.,1.,1.,
1.,1.,1.,1.,1.,1.,1.,1.,1.,1.,1.,1.,1.,1.,1.,1.,1.,1.,1.,1.,1.,1.,1.,1.,
1.,1.,1.,1.,1.,1.))
REPRESENTATION_ITEM('')
);
#69=(
BOUNDED_CURVE()
B_SPLINE_CURVE(5,(#22703,#22704,#22705,#22706,#22707,#22708,#22709,#22710,
#22711,#22712,#22713,#22714,#22715,#22716,#22717,#22718,#22719,#22720,#22721,
#22722,#22723,#22724,#22725,#22726,#22727,#22728,#22729,#22730,#22731,#22732,
#22733,#22734,#22735,#22736,#22737,#22738,#22739,#22740,#22741,#22742,#22743,
#22744,#22745,#22746,#22747,#22748,#22749,#22750,#22751,#22752,#22753,#22754,
#22755,#22756,#22757,#22758,#22759,#22760,#22761,#22762,#22763,#22764,#22765,
#22766,#22767,#22768,#22769,#22770,#22771,#22772),.UNSPECIFIED.,.F.,.F.)
B_SPLINE_CURVE_WITH_KNOTS((6,1,1,1,1,1,1,1,1,1,1,1,1,1,1,1,1,1,1,1,1,1,
1,1,1,1,1,1,1,1,1,1,1,1,1,1,1,1,1,1,1,1,1,1,1,1,1,1,1,1,1,1,1,1,1,1,1,1,
1,1,1,1,1,1,1,6),(0.,0.0153846153846154,0.0307692307692308,0.0461538461538462,
0.0615384615384615,0.0769230769230769,0.0923076923076923,0.107692307692308,
0.123076923076923,0.138461538461538,0.153846153846154,0.169230769230769,
0.184615384615385,0.2,0.215384615384615,0.230769230769231,0.246153846153846,
0.261538461538462,0.276923076923077,0.292307692307692,0.307692307692308,
0.323076923076923,0.338461538461538,0.353846153846154,0.369230769230769,
0.384615384615385,0.4,0.415384615384615,0.430769230769231,0.446153846153846,
0.461538461538462,0.476923076923077,0.492307692307692,0.507692307692308,
0.523076923076923,0.538461538461538,0.553846153846154,0.569230769230769,
0.584615384615384,0.6,0.615384615384615,0.63076923076923,0.646153846153846,
0.661538461538461,0.676923076923076,0.692307692307692,0.707692307692307,
0.723076923076922,0.738461538461538,0.753846153846153,0.769230769230768,
0.784615384615384,0.799999999999999,0.815384615384614,0.83076923076923,
0.846153846153845,0.86153846153846,0.876923076923076,0.892307692307691,
0.907692307692306,0.923076923076922,0.938461538461537,0.953846153846152,
0.969230769230768,0.984615384615383,1.),.UNSPECIFIED.)
CURVE()
GEOMETRIC_REPRESENTATION_ITEM()
RATIONAL_B_SPLINE_CURVE((1.,1.,1.,1.,1.,1.,1.,1.,1.,1.,1.,1.,1.,1.,1.,1.,
1.,1.,1.,1.,1.,1.,1.,1.,1.,1.,1.,1.,1.,1.,1.,1.,1.,1.,1.,1.,1.,1.,1.,1.,
1.,1.,1.,1.,1.,1.,1.,1.,1.,1.,1.,1.,1.,1.,1.,1.,1.,1.,1.,1.,1.,1.,1.,1.,
1.,1.,1.,1.,1.,1.))
REPRESENTATION_ITEM('')
);
#70=(
BOUNDED_CURVE()
B_SPLINE_CURVE(5,(#22776,#22777,#22778,#22779,#22780,#22781,#22782,#22783,
#22784,#22785,#22786,#22787,#22788,#22789,#22790,#22791,#22792,#22793,#22794,
#22795,#22796,#22797,#22798,#22799,#22800,#22801,#22802,#22803,#22804,#22805,
#22806,#22807,#22808,#22809,#22810,#22811,#22812,#22813,#22814,#22815,#22816,
#22817,#22818,#22819,#22820,#22821,#22822,#22823,#22824,#22825,#22826,#22827,
#22828,#22829,#22830,#22831,#22832,#22833,#22834,#22835,#22836,#22837,#22838,
#22839,#22840,#22841,#22842,#22843,#22844,#22845),.UNSPECIFIED.,.F.,.F.)
B_SPLINE_CURVE_WITH_KNOTS((6,1,1,1,1,1,1,1,1,1,1,1,1,1,1,1,1,1,1,1,1,1,
1,1,1,1,1,1,1,1,1,1,1,1,1,1,1,1,1,1,1,1,1,1,1,1,1,1,1,1,1,1,1,1,1,1,1,1,
1,1,1,1,1,1,1,6),(0.,0.0153846153846154,0.0307692307692308,0.0461538461538462,
0.0615384615384615,0.0769230769230769,0.0923076923076923,0.107692307692308,
0.123076923076923,0.138461538461538,0.153846153846154,0.169230769230769,
0.184615384615385,0.2,0.215384615384615,0.230769230769231,0.246153846153846,
0.261538461538462,0.276923076923077,0.292307692307692,0.307692307692308,
0.323076923076923,0.338461538461538,0.353846153846154,0.369230769230769,
0.384615384615385,0.4,0.415384615384615,0.430769230769231,0.446153846153846,
0.461538461538462,0.476923076923077,0.492307692307692,0.507692307692308,
0.523076923076923,0.538461538461538,0.553846153846154,0.569230769230769,
0.584615384615384,0.6,0.615384615384615,0.63076923076923,0.646153846153846,
0.661538461538461,0.676923076923076,0.692307692307692,0.707692307692307,
0.723076923076922,0.738461538461538,0.753846153846153,0.769230769230768,
0.784615384615384,0.799999999999999,0.815384615384614,0.83076923076923,
0.846153846153845,0.86153846153846,0.876923076923076,0.892307692307691,
0.907692307692306,0.923076923076922,0.938461538461537,0.953846153846152,
0.969230769230768,0.984615384615383,1.),.UNSPECIFIED.)
CURVE()
GEOMETRIC_REPRESENTATION_ITEM()
RATIONAL_B_SPLINE_CURVE((1.,1.,1.,1.,1.,1.,1.,1.,1.,1.,1.,1.,1.,1.,1.,1.,
1.,1.,1.,1.,1.,1.,1.,1.,1.,1.,1.,1.,1.,1.,1.,1.,1.,1.,1.,1.,1.,1.,1.,1.,
1.,1.,1.,1.,1.,1.,1.,1.,1.,1.,1.,1.,1.,1.,1.,1.,1.,1.,1.,1.,1.,1.,1.,1.,
1.,1.,1.,1.,1.,1.))
REPRESENTATION_ITEM('')
);
#71=(
BOUNDED_CURVE()
B_SPLINE_CURVE(5,(#22849,#22850,#22851,#22852,#22853,#22854,#22855,#22856,
#22857,#22858,#22859,#22860,#22861,#22862,#22863,#22864,#22865,#22866,#22867,
#22868,#22869,#22870,#22871,#22872,#22873,#22874,#22875,#22876,#22877,#22878,
#22879,#22880,#22881,#22882,#22883,#22884,#22885,#22886,#22887,#22888,#22889,
#22890,#22891,#22892,#22893,#22894,#22895,#22896,#22897,#22898,#22899,#22900,
#22901,#22902,#22903,#22904,#22905,#22906,#22907,#22908,#22909,#22910,#22911,
#22912,#22913,#22914,#22915,#22916,#22917,#22918),.UNSPECIFIED.,.F.,.F.)
B_SPLINE_CURVE_WITH_KNOTS((6,1,1,1,1,1,1,1,1,1,1,1,1,1,1,1,1,1,1,1,1,1,
1,1,1,1,1,1,1,1,1,1,1,1,1,1,1,1,1,1,1,1,1,1,1,1,1,1,1,1,1,1,1,1,1,1,1,1,
1,1,1,1,1,1,1,6),(0.,0.0153846153846154,0.0307692307692308,0.0461538461538462,
0.0615384615384615,0.0769230769230769,0.0923076923076923,0.107692307692308,
0.123076923076923,0.138461538461538,0.153846153846154,0.169230769230769,
0.184615384615385,0.2,0.215384615384615,0.230769230769231,0.246153846153846,
0.261538461538462,0.276923076923077,0.292307692307692,0.307692307692308,
0.323076923076923,0.338461538461538,0.353846153846154,0.369230769230769,
0.384615384615385,0.4,0.415384615384615,0.430769230769231,0.446153846153846,
0.461538461538462,0.476923076923077,0.492307692307692,0.507692307692308,
0.523076923076923,0.538461538461538,0.553846153846154,0.569230769230769,
0.584615384615384,0.6,0.615384615384615,0.63076923076923,0.646153846153846,
0.661538461538461,0.676923076923076,0.692307692307692,0.707692307692307,
0.723076923076922,0.738461538461538,0.753846153846153,0.769230769230768,
0.784615384615384,0.799999999999999,0.815384615384614,0.83076923076923,
0.846153846153845,0.86153846153846,0.876923076923076,0.892307692307691,
0.907692307692306,0.923076923076922,0.938461538461537,0.953846153846152,
0.969230769230768,0.984615384615383,1.),.UNSPECIFIED.)
CURVE()
GEOMETRIC_REPRESENTATION_ITEM()
RATIONAL_B_SPLINE_CURVE((1.,1.,1.,1.,1.,1.,1.,1.,1.,1.,1.,1.,1.,1.,1.,1.,
1.,1.,1.,1.,1.,1.,1.,1.,1.,1.,1.,1.,1.,1.,1.,1.,1.,1.,1.,1.,1.,1.,1.,1.,
1.,1.,1.,1.,1.,1.,1.,1.,1.,1.,1.,1.,1.,1.,1.,1.,1.,1.,1.,1.,1.,1.,1.,1.,
1.,1.,1.,1.,1.,1.))
REPRESENTATION_ITEM('')
);
#72=(
BOUNDED_CURVE()
B_SPLINE_CURVE(5,(#22922,#22923,#22924,#22925,#22926,#22927,#22928,#22929,
#22930,#22931,#22932,#22933,#22934,#22935,#22936,#22937,#22938,#22939,#22940,
#22941,#22942,#22943,#22944,#22945,#22946,#22947,#22948,#22949,#22950,#22951,
#22952,#22953,#22954,#22955,#22956,#22957,#22958,#22959,#22960,#22961,#22962,
#22963,#22964,#22965,#22966,#22967,#22968,#22969,#22970,#22971,#22972,#22973,
#22974,#22975,#22976,#22977,#22978,#22979,#22980,#22981,#22982,#22983,#22984,
#22985,#22986,#22987,#22988,#22989,#22990,#22991),.UNSPECIFIED.,.F.,.F.)
B_SPLINE_CURVE_WITH_KNOTS((6,1,1,1,1,1,1,1,1,1,1,1,1,1,1,1,1,1,1,1,1,1,
1,1,1,1,1,1,1,1,1,1,1,1,1,1,1,1,1,1,1,1,1,1,1,1,1,1,1,1,1,1,1,1,1,1,1,1,
1,1,1,1,1,1,1,6),(0.,0.0153846153846154,0.0307692307692308,0.0461538461538462,
0.0615384615384615,0.0769230769230769,0.0923076923076923,0.107692307692308,
0.123076923076923,0.138461538461538,0.153846153846154,0.169230769230769,
0.184615384615385,0.2,0.215384615384615,0.230769230769231,0.246153846153846,
0.261538461538462,0.276923076923077,0.292307692307692,0.307692307692308,
0.323076923076923,0.338461538461538,0.353846153846154,0.369230769230769,
0.384615384615385,0.4,0.415384615384615,0.430769230769231,0.446153846153846,
0.461538461538462,0.476923076923077,0.492307692307692,0.507692307692308,
0.523076923076923,0.538461538461538,0.553846153846154,0.569230769230769,
0.584615384615384,0.6,0.615384615384615,0.63076923076923,0.646153846153846,
0.661538461538461,0.676923076923076,0.692307692307692,0.707692307692307,
0.723076923076922,0.738461538461538,0.753846153846153,0.769230769230768,
0.784615384615384,0.799999999999999,0.815384615384614,0.83076923076923,
0.846153846153845,0.86153846153846,0.876923076923076,0.892307692307691,
0.907692307692306,0.923076923076922,0.938461538461537,0.953846153846152,
0.969230769230768,0.984615384615383,1.),.UNSPECIFIED.)
CURVE()
GEOMETRIC_REPRESENTATION_ITEM()
RATIONAL_B_SPLINE_CURVE((1.,1.,1.,1.,1.,1.,1.,1.,1.,1.,1.,1.,1.,1.,1.,1.,
1.,1.,1.,1.,1.,1.,1.,1.,1.,1.,1.,1.,1.,1.,1.,1.,1.,1.,1.,1.,1.,1.,1.,1.,
1.,1.,1.,1.,1.,1.,1.,1.,1.,1.,1.,1.,1.,1.,1.,1.,1.,1.,1.,1.,1.,1.,1.,1.,
1.,1.,1.,1.,1.,1.))
REPRESENTATION_ITEM('')
);
#73=(
BOUNDED_CURVE()
B_SPLINE_CURVE(5,(#22995,#22996,#22997,#22998,#22999,#23000,#23001,#23002,
#23003,#23004,#23005,#23006,#23007,#23008,#23009,#23010,#23011,#23012,#23013,
#23014,#23015,#23016,#23017,#23018,#23019,#23020,#23021,#23022,#23023,#23024,
#23025,#23026,#23027,#23028,#23029,#23030,#23031,#23032,#23033,#23034,#23035,
#23036,#23037,#23038,#23039,#23040,#23041,#23042,#23043,#23044,#23045,#23046,
#23047,#23048,#23049,#23050,#23051,#23052,#23053,#23054,#23055,#23056,#23057,
#23058,#23059,#23060,#23061,#23062,#23063,#23064),.UNSPECIFIED.,.F.,.F.)
B_SPLINE_CURVE_WITH_KNOTS((6,1,1,1,1,1,1,1,1,1,1,1,1,1,1,1,1,1,1,1,1,1,
1,1,1,1,1,1,1,1,1,1,1,1,1,1,1,1,1,1,1,1,1,1,1,1,1,1,1,1,1,1,1,1,1,1,1,1,
1,1,1,1,1,1,1,6),(0.,0.0153846153846154,0.0307692307692308,0.0461538461538462,
0.0615384615384615,0.0769230769230769,0.0923076923076923,0.107692307692308,
0.123076923076923,0.138461538461538,0.153846153846154,0.169230769230769,
0.184615384615385,0.2,0.215384615384615,0.230769230769231,0.246153846153846,
0.261538461538462,0.276923076923077,0.292307692307692,0.307692307692308,
0.323076923076923,0.338461538461538,0.353846153846154,0.369230769230769,
0.384615384615385,0.4,0.415384615384615,0.430769230769231,0.446153846153846,
0.461538461538462,0.476923076923077,0.492307692307692,0.507692307692308,
0.523076923076923,0.538461538461538,0.553846153846154,0.569230769230769,
0.584615384615384,0.6,0.615384615384615,0.63076923076923,0.646153846153846,
0.661538461538461,0.676923076923076,0.692307692307692,0.707692307692307,
0.723076923076922,0.738461538461538,0.753846153846153,0.769230769230768,
0.784615384615384,0.799999999999999,0.815384615384614,0.83076923076923,
0.846153846153845,0.86153846153846,0.876923076923076,0.892307692307691,
0.907692307692306,0.923076923076922,0.938461538461537,0.953846153846152,
0.969230769230768,0.984615384615383,1.),.UNSPECIFIED.)
CURVE()
GEOMETRIC_REPRESENTATION_ITEM()
RATIONAL_B_SPLINE_CURVE((1.,1.,1.,1.,1.,1.,1.,1.,1.,1.,1.,1.,1.,1.,1.,1.,
1.,1.,1.,1.,1.,1.,1.,1.,1.,1.,1.,1.,1.,1.,1.,1.,1.,1.,1.,1.,1.,1.,1.,1.,
1.,1.,1.,1.,1.,1.,1.,1.,1.,1.,1.,1.,1.,1.,1.,1.,1.,1.,1.,1.,1.,1.,1.,1.,
1.,1.,1.,1.,1.,1.))
REPRESENTATION_ITEM('')
);
#74=(
BOUNDED_CURVE()
B_SPLINE_CURVE(5,(#23068,#23069,#23070,#23071,#23072,#23073,#23074,#23075,
#23076,#23077,#23078,#23079,#23080,#23081,#23082,#23083,#23084,#23085,#23086,
#23087,#23088,#23089,#23090,#23091,#23092,#23093,#23094,#23095,#23096,#23097,
#23098,#23099,#23100,#23101,#23102,#23103,#23104,#23105,#23106,#23107,#23108,
#23109,#23110,#23111,#23112,#23113,#23114,#23115,#23116,#23117,#23118,#23119,
#23120,#23121,#23122,#23123,#23124,#23125,#23126,#23127,#23128,#23129,#23130,
#23131,#23132,#23133,#23134,#23135,#23136,#23137),.UNSPECIFIED.,.F.,.F.)
B_SPLINE_CURVE_WITH_KNOTS((6,1,1,1,1,1,1,1,1,1,1,1,1,1,1,1,1,1,1,1,1,1,
1,1,1,1,1,1,1,1,1,1,1,1,1,1,1,1,1,1,1,1,1,1,1,1,1,1,1,1,1,1,1,1,1,1,1,1,
1,1,1,1,1,1,1,6),(0.,0.0153846153846154,0.0307692307692308,0.0461538461538462,
0.0615384615384615,0.0769230769230769,0.0923076923076923,0.107692307692308,
0.123076923076923,0.138461538461538,0.153846153846154,0.169230769230769,
0.184615384615385,0.2,0.215384615384615,0.230769230769231,0.246153846153846,
0.261538461538462,0.276923076923077,0.292307692307692,0.307692307692308,
0.323076923076923,0.338461538461538,0.353846153846154,0.369230769230769,
0.384615384615385,0.4,0.415384615384615,0.430769230769231,0.446153846153846,
0.461538461538462,0.476923076923077,0.492307692307692,0.507692307692308,
0.523076923076923,0.538461538461538,0.553846153846154,0.569230769230769,
0.584615384615384,0.6,0.615384615384615,0.63076923076923,0.646153846153846,
0.661538461538461,0.676923076923076,0.692307692307692,0.707692307692307,
0.723076923076922,0.738461538461538,0.753846153846153,0.769230769230768,
0.784615384615384,0.799999999999999,0.815384615384614,0.83076923076923,
0.846153846153845,0.86153846153846,0.876923076923076,0.892307692307691,
0.907692307692306,0.923076923076922,0.938461538461537,0.953846153846152,
0.969230769230768,0.984615384615383,1.),.UNSPECIFIED.)
CURVE()
GEOMETRIC_REPRESENTATION_ITEM()
RATIONAL_B_SPLINE_CURVE((1.,1.,1.,1.,1.,1.,1.,1.,1.,1.,1.,1.,1.,1.,1.,1.,
1.,1.,1.,1.,1.,1.,1.,1.,1.,1.,1.,1.,1.,1.,1.,1.,1.,1.,1.,1.,1.,1.,1.,1.,
1.,1.,1.,1.,1.,1.,1.,1.,1.,1.,1.,1.,1.,1.,1.,1.,1.,1.,1.,1.,1.,1.,1.,1.,
1.,1.,1.,1.,1.,1.))
REPRESENTATION_ITEM('')
);
#75=(
BOUNDED_CURVE()
B_SPLINE_CURVE(5,(#23141,#23142,#23143,#23144,#23145,#23146,#23147,#23148,
#23149,#23150,#23151,#23152,#23153,#23154,#23155,#23156,#23157,#23158,#23159,
#23160,#23161,#23162,#23163,#23164,#23165,#23166,#23167,#23168,#23169,#23170,
#23171,#23172,#23173,#23174,#23175,#23176,#23177,#23178,#23179,#23180,#23181,
#23182,#23183,#23184,#23185,#23186,#23187,#23188,#23189,#23190,#23191,#23192,
#23193,#23194,#23195,#23196,#23197,#23198,#23199,#23200,#23201,#23202,#23203,
#23204,#23205,#23206,#23207,#23208,#23209,#23210),.UNSPECIFIED.,.F.,.F.)
B_SPLINE_CURVE_WITH_KNOTS((6,1,1,1,1,1,1,1,1,1,1,1,1,1,1,1,1,1,1,1,1,1,
1,1,1,1,1,1,1,1,1,1,1,1,1,1,1,1,1,1,1,1,1,1,1,1,1,1,1,1,1,1,1,1,1,1,1,1,
1,1,1,1,1,1,1,6),(0.,0.0153846153846154,0.0307692307692308,0.0461538461538462,
0.0615384615384615,0.0769230769230769,0.0923076923076923,0.107692307692308,
0.123076923076923,0.138461538461538,0.153846153846154,0.169230769230769,
0.184615384615385,0.2,0.215384615384615,0.230769230769231,0.246153846153846,
0.261538461538462,0.276923076923077,0.292307692307692,0.307692307692308,
0.323076923076923,0.338461538461538,0.353846153846154,0.369230769230769,
0.384615384615385,0.4,0.415384615384615,0.430769230769231,0.446153846153846,
0.461538461538462,0.476923076923077,0.492307692307692,0.507692307692308,
0.523076923076923,0.538461538461538,0.553846153846154,0.569230769230769,
0.584615384615384,0.6,0.615384615384615,0.63076923076923,0.646153846153846,
0.661538461538461,0.676923076923076,0.692307692307692,0.707692307692307,
0.723076923076922,0.738461538461538,0.753846153846153,0.769230769230768,
0.784615384615384,0.799999999999999,0.815384615384614,0.83076923076923,
0.846153846153845,0.86153846153846,0.876923076923076,0.892307692307691,
0.907692307692306,0.923076923076922,0.938461538461537,0.953846153846152,
0.969230769230768,0.984615384615383,1.),.UNSPECIFIED.)
CURVE()
GEOMETRIC_REPRESENTATION_ITEM()
RATIONAL_B_SPLINE_CURVE((1.,1.,1.,1.,1.,1.,1.,1.,1.,1.,1.,1.,1.,1.,1.,1.,
1.,1.,1.,1.,1.,1.,1.,1.,1.,1.,1.,1.,1.,1.,1.,1.,1.,1.,1.,1.,1.,1.,1.,1.,
1.,1.,1.,1.,1.,1.,1.,1.,1.,1.,1.,1.,1.,1.,1.,1.,1.,1.,1.,1.,1.,1.,1.,1.,
1.,1.,1.,1.,1.,1.))
REPRESENTATION_ITEM('')
);
#76=(
BOUNDED_CURVE()
B_SPLINE_CURVE(5,(#23214,#23215,#23216,#23217,#23218,#23219,#23220,#23221,
#23222,#23223,#23224,#23225,#23226,#23227,#23228,#23229,#23230,#23231,#23232,
#23233,#23234,#23235,#23236,#23237,#23238,#23239,#23240,#23241,#23242,#23243,
#23244,#23245,#23246,#23247,#23248,#23249,#23250,#23251,#23252,#23253,#23254,
#23255,#23256,#23257,#23258,#23259,#23260,#23261,#23262,#23263,#23264,#23265,
#23266,#23267,#23268,#23269,#23270,#23271,#23272,#23273,#23274,#23275,#23276,
#23277,#23278,#23279,#23280,#23281,#23282,#23283),.UNSPECIFIED.,.F.,.F.)
B_SPLINE_CURVE_WITH_KNOTS((6,1,1,1,1,1,1,1,1,1,1,1,1,1,1,1,1,1,1,1,1,1,
1,1,1,1,1,1,1,1,1,1,1,1,1,1,1,1,1,1,1,1,1,1,1,1,1,1,1,1,1,1,1,1,1,1,1,1,
1,1,1,1,1,1,1,6),(0.,0.0153846153846154,0.0307692307692308,0.0461538461538462,
0.0615384615384615,0.0769230769230769,0.0923076923076923,0.107692307692308,
0.123076923076923,0.138461538461538,0.153846153846154,0.169230769230769,
0.184615384615385,0.2,0.215384615384615,0.230769230769231,0.246153846153846,
0.261538461538462,0.276923076923077,0.292307692307692,0.307692307692308,
0.323076923076923,0.338461538461538,0.353846153846154,0.369230769230769,
0.384615384615385,0.4,0.415384615384615,0.430769230769231,0.446153846153846,
0.461538461538462,0.476923076923077,0.492307692307692,0.507692307692308,
0.523076923076923,0.538461538461538,0.553846153846154,0.569230769230769,
0.584615384615384,0.6,0.615384615384615,0.63076923076923,0.646153846153846,
0.661538461538461,0.676923076923076,0.692307692307692,0.707692307692307,
0.723076923076922,0.738461538461538,0.753846153846153,0.769230769230768,
0.784615384615384,0.799999999999999,0.815384615384614,0.83076923076923,
0.846153846153845,0.86153846153846,0.876923076923076,0.892307692307691,
0.907692307692306,0.923076923076922,0.938461538461537,0.953846153846152,
0.969230769230768,0.984615384615383,1.),.UNSPECIFIED.)
CURVE()
GEOMETRIC_REPRESENTATION_ITEM()
RATIONAL_B_SPLINE_CURVE((1.,1.,1.,1.,1.,1.,1.,1.,1.,1.,1.,1.,1.,1.,1.,1.,
1.,1.,1.,1.,1.,1.,1.,1.,1.,1.,1.,1.,1.,1.,1.,1.,1.,1.,1.,1.,1.,1.,1.,1.,
1.,1.,1.,1.,1.,1.,1.,1.,1.,1.,1.,1.,1.,1.,1.,1.,1.,1.,1.,1.,1.,1.,1.,1.,
1.,1.,1.,1.,1.,1.))
REPRESENTATION_ITEM('')
);
#77=(
BOUNDED_CURVE()
B_SPLINE_CURVE(5,(#23287,#23288,#23289,#23290,#23291,#23292,#23293,#23294,
#23295,#23296,#23297,#23298,#23299,#23300,#23301,#23302,#23303,#23304,#23305,
#23306,#23307,#23308,#23309,#23310,#23311,#23312,#23313,#23314,#23315,#23316,
#23317,#23318,#23319,#23320,#23321,#23322,#23323,#23324,#23325,#23326,#23327,
#23328,#23329,#23330,#23331,#23332,#23333,#23334,#23335,#23336,#23337,#23338,
#23339,#23340,#23341,#23342,#23343,#23344,#23345,#23346,#23347,#23348,#23349,
#23350,#23351,#23352,#23353,#23354,#23355,#23356),.UNSPECIFIED.,.F.,.F.)
B_SPLINE_CURVE_WITH_KNOTS((6,1,1,1,1,1,1,1,1,1,1,1,1,1,1,1,1,1,1,1,1,1,
1,1,1,1,1,1,1,1,1,1,1,1,1,1,1,1,1,1,1,1,1,1,1,1,1,1,1,1,1,1,1,1,1,1,1,1,
1,1,1,1,1,1,1,6),(0.,0.0153846153846154,0.0307692307692308,0.0461538461538462,
0.0615384615384615,0.0769230769230769,0.0923076923076923,0.107692307692308,
0.123076923076923,0.138461538461538,0.153846153846154,0.169230769230769,
0.184615384615385,0.2,0.215384615384615,0.230769230769231,0.246153846153846,
0.261538461538462,0.276923076923077,0.292307692307692,0.307692307692308,
0.323076923076923,0.338461538461538,0.353846153846154,0.369230769230769,
0.384615384615385,0.4,0.415384615384615,0.430769230769231,0.446153846153846,
0.461538461538462,0.476923076923077,0.492307692307692,0.507692307692308,
0.523076923076923,0.538461538461538,0.553846153846154,0.569230769230769,
0.584615384615384,0.6,0.615384615384615,0.63076923076923,0.646153846153846,
0.661538461538461,0.676923076923076,0.692307692307692,0.707692307692307,
0.723076923076922,0.738461538461538,0.753846153846153,0.769230769230768,
0.784615384615384,0.799999999999999,0.815384615384614,0.83076923076923,
0.846153846153845,0.86153846153846,0.876923076923076,0.892307692307691,
0.907692307692306,0.923076923076922,0.938461538461537,0.953846153846152,
0.969230769230768,0.984615384615383,1.),.UNSPECIFIED.)
CURVE()
GEOMETRIC_REPRESENTATION_ITEM()
RATIONAL_B_SPLINE_CURVE((1.,1.,1.,1.,1.,1.,1.,1.,1.,1.,1.,1.,1.,1.,1.,1.,
1.,1.,1.,1.,1.,1.,1.,1.,1.,1.,1.,1.,1.,1.,1.,1.,1.,1.,1.,1.,1.,1.,1.,1.,
1.,1.,1.,1.,1.,1.,1.,1.,1.,1.,1.,1.,1.,1.,1.,1.,1.,1.,1.,1.,1.,1.,1.,1.,
1.,1.,1.,1.,1.,1.))
REPRESENTATION_ITEM('')
);
#78=(
BOUNDED_CURVE()
B_SPLINE_CURVE(5,(#23360,#23361,#23362,#23363,#23364,#23365,#23366,#23367,
#23368,#23369,#23370,#23371,#23372,#23373,#23374,#23375,#23376,#23377,#23378,
#23379,#23380,#23381,#23382,#23383,#23384,#23385,#23386,#23387,#23388,#23389,
#23390,#23391,#23392,#23393,#23394,#23395,#23396,#23397,#23398,#23399,#23400,
#23401,#23402,#23403,#23404,#23405,#23406,#23407,#23408,#23409,#23410,#23411,
#23412,#23413,#23414,#23415,#23416,#23417,#23418,#23419,#23420,#23421,#23422,
#23423,#23424,#23425,#23426,#23427,#23428,#23429),.UNSPECIFIED.,.F.,.F.)
B_SPLINE_CURVE_WITH_KNOTS((6,1,1,1,1,1,1,1,1,1,1,1,1,1,1,1,1,1,1,1,1,1,
1,1,1,1,1,1,1,1,1,1,1,1,1,1,1,1,1,1,1,1,1,1,1,1,1,1,1,1,1,1,1,1,1,1,1,1,
1,1,1,1,1,1,1,6),(0.,0.0153846153846154,0.0307692307692308,0.0461538461538462,
0.0615384615384615,0.0769230769230769,0.0923076923076923,0.107692307692308,
0.123076923076923,0.138461538461538,0.153846153846154,0.169230769230769,
0.184615384615385,0.2,0.215384615384615,0.230769230769231,0.246153846153846,
0.261538461538462,0.276923076923077,0.292307692307692,0.307692307692308,
0.323076923076923,0.338461538461538,0.353846153846154,0.369230769230769,
0.384615384615385,0.4,0.415384615384615,0.430769230769231,0.446153846153846,
0.461538461538462,0.476923076923077,0.492307692307692,0.507692307692308,
0.523076923076923,0.538461538461538,0.553846153846154,0.569230769230769,
0.584615384615384,0.6,0.615384615384615,0.63076923076923,0.646153846153846,
0.661538461538461,0.676923076923076,0.692307692307692,0.707692307692307,
0.723076923076922,0.738461538461538,0.753846153846153,0.769230769230768,
0.784615384615384,0.799999999999999,0.815384615384614,0.83076923076923,
0.846153846153845,0.86153846153846,0.876923076923076,0.892307692307691,
0.907692307692306,0.923076923076922,0.938461538461537,0.953846153846152,
0.969230769230768,0.984615384615383,1.),.UNSPECIFIED.)
CURVE()
GEOMETRIC_REPRESENTATION_ITEM()
RATIONAL_B_SPLINE_CURVE((1.,1.,1.,1.,1.,1.,1.,1.,1.,1.,1.,1.,1.,1.,1.,1.,
1.,1.,1.,1.,1.,1.,1.,1.,1.,1.,1.,1.,1.,1.,1.,1.,1.,1.,1.,1.,1.,1.,1.,1.,
1.,1.,1.,1.,1.,1.,1.,1.,1.,1.,1.,1.,1.,1.,1.,1.,1.,1.,1.,1.,1.,1.,1.,1.,
1.,1.,1.,1.,1.,1.))
REPRESENTATION_ITEM('')
);
#79=(
BOUNDED_CURVE()
B_SPLINE_CURVE(5,(#23433,#23434,#23435,#23436,#23437,#23438,#23439,#23440,
#23441,#23442,#23443,#23444,#23445,#23446,#23447,#23448,#23449,#23450,#23451,
#23452,#23453,#23454,#23455,#23456,#23457,#23458,#23459,#23460,#23461,#23462,
#23463,#23464,#23465,#23466,#23467,#23468,#23469,#23470,#23471,#23472,#23473,
#23474,#23475,#23476,#23477,#23478,#23479,#23480,#23481,#23482,#23483,#23484,
#23485,#23486,#23487,#23488,#23489,#23490,#23491,#23492,#23493,#23494,#23495,
#23496,#23497,#23498,#23499,#23500,#23501,#23502),.UNSPECIFIED.,.F.,.F.)
B_SPLINE_CURVE_WITH_KNOTS((6,1,1,1,1,1,1,1,1,1,1,1,1,1,1,1,1,1,1,1,1,1,
1,1,1,1,1,1,1,1,1,1,1,1,1,1,1,1,1,1,1,1,1,1,1,1,1,1,1,1,1,1,1,1,1,1,1,1,
1,1,1,1,1,1,1,6),(0.,0.0153846153846154,0.0307692307692308,0.0461538461538462,
0.0615384615384615,0.0769230769230769,0.0923076923076923,0.107692307692308,
0.123076923076923,0.138461538461538,0.153846153846154,0.169230769230769,
0.184615384615385,0.2,0.215384615384615,0.230769230769231,0.246153846153846,
0.261538461538462,0.276923076923077,0.292307692307692,0.307692307692308,
0.323076923076923,0.338461538461538,0.353846153846154,0.369230769230769,
0.384615384615385,0.4,0.415384615384615,0.430769230769231,0.446153846153846,
0.461538461538462,0.476923076923077,0.492307692307692,0.507692307692308,
0.523076923076923,0.538461538461538,0.553846153846154,0.569230769230769,
0.584615384615384,0.6,0.615384615384615,0.63076923076923,0.646153846153846,
0.661538461538461,0.676923076923076,0.692307692307692,0.707692307692307,
0.723076923076922,0.738461538461538,0.753846153846153,0.769230769230768,
0.784615384615384,0.799999999999999,0.815384615384614,0.83076923076923,
0.846153846153845,0.86153846153846,0.876923076923076,0.892307692307691,
0.907692307692306,0.923076923076922,0.938461538461537,0.953846153846152,
0.969230769230768,0.984615384615383,1.),.UNSPECIFIED.)
CURVE()
GEOMETRIC_REPRESENTATION_ITEM()
RATIONAL_B_SPLINE_CURVE((1.,1.,1.,1.,1.,1.,1.,1.,1.,1.,1.,1.,1.,1.,1.,1.,
1.,1.,1.,1.,1.,1.,1.,1.,1.,1.,1.,1.,1.,1.,1.,1.,1.,1.,1.,1.,1.,1.,1.,1.,
1.,1.,1.,1.,1.,1.,1.,1.,1.,1.,1.,1.,1.,1.,1.,1.,1.,1.,1.,1.,1.,1.,1.,1.,
1.,1.,1.,1.,1.,1.))
REPRESENTATION_ITEM('')
);
#80=(
BOUNDED_CURVE()
B_SPLINE_CURVE(5,(#23506,#23507,#23508,#23509,#23510,#23511,#23512,#23513,
#23514,#23515,#23516,#23517,#23518,#23519,#23520,#23521,#23522,#23523,#23524,
#23525,#23526,#23527,#23528,#23529,#23530,#23531,#23532,#23533,#23534,#23535,
#23536,#23537,#23538,#23539,#23540,#23541,#23542,#23543,#23544,#23545,#23546,
#23547,#23548,#23549,#23550,#23551,#23552,#23553,#23554,#23555,#23556,#23557,
#23558,#23559,#23560,#23561,#23562,#23563,#23564,#23565,#23566,#23567,#23568,
#23569,#23570,#23571,#23572,#23573,#23574,#23575),.UNSPECIFIED.,.F.,.F.)
B_SPLINE_CURVE_WITH_KNOTS((6,1,1,1,1,1,1,1,1,1,1,1,1,1,1,1,1,1,1,1,1,1,
1,1,1,1,1,1,1,1,1,1,1,1,1,1,1,1,1,1,1,1,1,1,1,1,1,1,1,1,1,1,1,1,1,1,1,1,
1,1,1,1,1,1,1,6),(0.,0.0153846153846154,0.0307692307692308,0.0461538461538462,
0.0615384615384615,0.0769230769230769,0.0923076923076923,0.107692307692308,
0.123076923076923,0.138461538461538,0.153846153846154,0.169230769230769,
0.184615384615385,0.2,0.215384615384615,0.230769230769231,0.246153846153846,
0.261538461538462,0.276923076923077,0.292307692307692,0.307692307692308,
0.323076923076923,0.338461538461538,0.353846153846154,0.369230769230769,
0.384615384615385,0.4,0.415384615384615,0.430769230769231,0.446153846153846,
0.461538461538462,0.476923076923077,0.492307692307692,0.507692307692308,
0.523076923076923,0.538461538461538,0.553846153846154,0.569230769230769,
0.584615384615384,0.6,0.615384615384615,0.63076923076923,0.646153846153846,
0.661538461538461,0.676923076923076,0.692307692307692,0.707692307692307,
0.723076923076922,0.738461538461538,0.753846153846153,0.769230769230768,
0.784615384615384,0.799999999999999,0.815384615384614,0.83076923076923,
0.846153846153845,0.86153846153846,0.876923076923076,0.892307692307691,
0.907692307692306,0.923076923076922,0.938461538461537,0.953846153846152,
0.969230769230768,0.984615384615383,1.),.UNSPECIFIED.)
CURVE()
GEOMETRIC_REPRESENTATION_ITEM()
RATIONAL_B_SPLINE_CURVE((1.,1.,1.,1.,1.,1.,1.,1.,1.,1.,1.,1.,1.,1.,1.,1.,
1.,1.,1.,1.,1.,1.,1.,1.,1.,1.,1.,1.,1.,1.,1.,1.,1.,1.,1.,1.,1.,1.,1.,1.,
1.,1.,1.,1.,1.,1.,1.,1.,1.,1.,1.,1.,1.,1.,1.,1.,1.,1.,1.,1.,1.,1.,1.,1.,
1.,1.,1.,1.,1.,1.))
REPRESENTATION_ITEM('')
);
#81=(
BOUNDED_CURVE()
B_SPLINE_CURVE(5,(#23579,#23580,#23581,#23582,#23583,#23584,#23585,#23586,
#23587,#23588,#23589,#23590,#23591,#23592,#23593,#23594,#23595,#23596,#23597,
#23598,#23599,#23600,#23601,#23602,#23603,#23604,#23605,#23606,#23607,#23608,
#23609,#23610,#23611,#23612,#23613,#23614,#23615,#23616,#23617,#23618,#23619,
#23620,#23621,#23622,#23623,#23624,#23625,#23626,#23627,#23628,#23629,#23630,
#23631,#23632,#23633,#23634,#23635,#23636,#23637,#23638,#23639,#23640,#23641,
#23642,#23643,#23644,#23645,#23646,#23647,#23648),.UNSPECIFIED.,.F.,.F.)
B_SPLINE_CURVE_WITH_KNOTS((6,1,1,1,1,1,1,1,1,1,1,1,1,1,1,1,1,1,1,1,1,1,
1,1,1,1,1,1,1,1,1,1,1,1,1,1,1,1,1,1,1,1,1,1,1,1,1,1,1,1,1,1,1,1,1,1,1,1,
1,1,1,1,1,1,1,6),(0.,0.0153846153846154,0.0307692307692308,0.0461538461538462,
0.0615384615384615,0.0769230769230769,0.0923076923076923,0.107692307692308,
0.123076923076923,0.138461538461538,0.153846153846154,0.169230769230769,
0.184615384615385,0.2,0.215384615384615,0.230769230769231,0.246153846153846,
0.261538461538462,0.276923076923077,0.292307692307692,0.307692307692308,
0.323076923076923,0.338461538461538,0.353846153846154,0.369230769230769,
0.384615384615385,0.4,0.415384615384615,0.430769230769231,0.446153846153846,
0.461538461538462,0.476923076923077,0.492307692307692,0.507692307692308,
0.523076923076923,0.538461538461538,0.553846153846154,0.569230769230769,
0.584615384615384,0.6,0.615384615384615,0.63076923076923,0.646153846153846,
0.661538461538461,0.676923076923076,0.692307692307692,0.707692307692307,
0.723076923076922,0.738461538461538,0.753846153846153,0.769230769230768,
0.784615384615384,0.799999999999999,0.815384615384614,0.83076923076923,
0.846153846153845,0.86153846153846,0.876923076923076,0.892307692307691,
0.907692307692306,0.923076923076922,0.938461538461537,0.953846153846152,
0.969230769230768,0.984615384615383,1.),.UNSPECIFIED.)
CURVE()
GEOMETRIC_REPRESENTATION_ITEM()
RATIONAL_B_SPLINE_CURVE((1.,1.,1.,1.,1.,1.,1.,1.,1.,1.,1.,1.,1.,1.,1.,1.,
1.,1.,1.,1.,1.,1.,1.,1.,1.,1.,1.,1.,1.,1.,1.,1.,1.,1.,1.,1.,1.,1.,1.,1.,
1.,1.,1.,1.,1.,1.,1.,1.,1.,1.,1.,1.,1.,1.,1.,1.,1.,1.,1.,1.,1.,1.,1.,1.,
1.,1.,1.,1.,1.,1.))
REPRESENTATION_ITEM('')
);
#82=(
BOUNDED_CURVE()
B_SPLINE_CURVE(5,(#23652,#23653,#23654,#23655,#23656,#23657,#23658,#23659,
#23660,#23661,#23662,#23663,#23664,#23665,#23666,#23667,#23668,#23669,#23670,
#23671,#23672,#23673,#23674,#23675,#23676,#23677,#23678,#23679,#23680,#23681,
#23682,#23683,#23684,#23685,#23686,#23687,#23688,#23689,#23690,#23691,#23692,
#23693,#23694,#23695,#23696,#23697,#23698,#23699,#23700,#23701,#23702,#23703,
#23704,#23705,#23706,#23707,#23708,#23709,#23710,#23711,#23712,#23713,#23714,
#23715,#23716,#23717,#23718,#23719,#23720,#23721),.UNSPECIFIED.,.F.,.F.)
B_SPLINE_CURVE_WITH_KNOTS((6,1,1,1,1,1,1,1,1,1,1,1,1,1,1,1,1,1,1,1,1,1,
1,1,1,1,1,1,1,1,1,1,1,1,1,1,1,1,1,1,1,1,1,1,1,1,1,1,1,1,1,1,1,1,1,1,1,1,
1,1,1,1,1,1,1,6),(0.,0.0153846153846154,0.0307692307692308,0.0461538461538462,
0.0615384615384615,0.0769230769230769,0.0923076923076923,0.107692307692308,
0.123076923076923,0.138461538461538,0.153846153846154,0.169230769230769,
0.184615384615385,0.2,0.215384615384615,0.230769230769231,0.246153846153846,
0.261538461538462,0.276923076923077,0.292307692307692,0.307692307692308,
0.323076923076923,0.338461538461538,0.353846153846154,0.369230769230769,
0.384615384615385,0.4,0.415384615384615,0.430769230769231,0.446153846153846,
0.461538461538462,0.476923076923077,0.492307692307692,0.507692307692308,
0.523076923076923,0.538461538461538,0.553846153846154,0.569230769230769,
0.584615384615384,0.6,0.615384615384615,0.63076923076923,0.646153846153846,
0.661538461538461,0.676923076923076,0.692307692307692,0.707692307692307,
0.723076923076922,0.738461538461538,0.753846153846153,0.769230769230768,
0.784615384615384,0.799999999999999,0.815384615384614,0.83076923076923,
0.846153846153845,0.86153846153846,0.876923076923076,0.892307692307691,
0.907692307692306,0.923076923076922,0.938461538461537,0.953846153846152,
0.969230769230768,0.984615384615383,1.),.UNSPECIFIED.)
CURVE()
GEOMETRIC_REPRESENTATION_ITEM()
RATIONAL_B_SPLINE_CURVE((1.,1.,1.,1.,1.,1.,1.,1.,1.,1.,1.,1.,1.,1.,1.,1.,
1.,1.,1.,1.,1.,1.,1.,1.,1.,1.,1.,1.,1.,1.,1.,1.,1.,1.,1.,1.,1.,1.,1.,1.,
1.,1.,1.,1.,1.,1.,1.,1.,1.,1.,1.,1.,1.,1.,1.,1.,1.,1.,1.,1.,1.,1.,1.,1.,
1.,1.,1.,1.,1.,1.))
REPRESENTATION_ITEM('')
);
#83=(
BOUNDED_CURVE()
B_SPLINE_CURVE(5,(#23725,#23726,#23727,#23728,#23729,#23730,#23731,#23732,
#23733,#23734,#23735,#23736,#23737,#23738,#23739,#23740,#23741,#23742,#23743,
#23744,#23745,#23746,#23747,#23748,#23749,#23750,#23751,#23752,#23753,#23754,
#23755,#23756,#23757,#23758,#23759,#23760,#23761,#23762,#23763,#23764,#23765,
#23766,#23767,#23768,#23769,#23770,#23771,#23772,#23773,#23774,#23775,#23776,
#23777,#23778,#23779,#23780,#23781,#23782,#23783,#23784,#23785,#23786,#23787,
#23788,#23789,#23790,#23791,#23792,#23793,#23794),.UNSPECIFIED.,.F.,.F.)
B_SPLINE_CURVE_WITH_KNOTS((6,1,1,1,1,1,1,1,1,1,1,1,1,1,1,1,1,1,1,1,1,1,
1,1,1,1,1,1,1,1,1,1,1,1,1,1,1,1,1,1,1,1,1,1,1,1,1,1,1,1,1,1,1,1,1,1,1,1,
1,1,1,1,1,1,1,6),(0.,0.0153846153846154,0.0307692307692308,0.0461538461538462,
0.0615384615384615,0.0769230769230769,0.0923076923076923,0.107692307692308,
0.123076923076923,0.138461538461538,0.153846153846154,0.169230769230769,
0.184615384615385,0.2,0.215384615384615,0.230769230769231,0.246153846153846,
0.261538461538462,0.276923076923077,0.292307692307692,0.307692307692308,
0.323076923076923,0.338461538461538,0.353846153846154,0.369230769230769,
0.384615384615385,0.4,0.415384615384615,0.430769230769231,0.446153846153846,
0.461538461538462,0.476923076923077,0.492307692307692,0.507692307692308,
0.523076923076923,0.538461538461538,0.553846153846154,0.569230769230769,
0.584615384615384,0.6,0.615384615384615,0.63076923076923,0.646153846153846,
0.661538461538461,0.676923076923076,0.692307692307692,0.707692307692307,
0.723076923076922,0.738461538461538,0.753846153846153,0.769230769230768,
0.784615384615384,0.799999999999999,0.815384615384614,0.83076923076923,
0.846153846153845,0.86153846153846,0.876923076923076,0.892307692307691,
0.907692307692306,0.923076923076922,0.938461538461537,0.953846153846152,
0.969230769230768,0.984615384615383,1.),.UNSPECIFIED.)
CURVE()
GEOMETRIC_REPRESENTATION_ITEM()
RATIONAL_B_SPLINE_CURVE((1.,1.,1.,1.,1.,1.,1.,1.,1.,1.,1.,1.,1.,1.,1.,1.,
1.,1.,1.,1.,1.,1.,1.,1.,1.,1.,1.,1.,1.,1.,1.,1.,1.,1.,1.,1.,1.,1.,1.,1.,
1.,1.,1.,1.,1.,1.,1.,1.,1.,1.,1.,1.,1.,1.,1.,1.,1.,1.,1.,1.,1.,1.,1.,1.,
1.,1.,1.,1.,1.,1.))
REPRESENTATION_ITEM('')
);
#84=(
BOUNDED_CURVE()
B_SPLINE_CURVE(5,(#23798,#23799,#23800,#23801,#23802,#23803,#23804,#23805,
#23806,#23807,#23808,#23809,#23810,#23811,#23812,#23813,#23814,#23815,#23816,
#23817,#23818,#23819,#23820,#23821,#23822,#23823,#23824,#23825,#23826,#23827,
#23828,#23829,#23830,#23831,#23832,#23833,#23834,#23835,#23836,#23837,#23838,
#23839,#23840,#23841,#23842,#23843,#23844,#23845,#23846,#23847,#23848,#23849,
#23850,#23851,#23852,#23853,#23854,#23855,#23856,#23857,#23858,#23859,#23860,
#23861,#23862,#23863,#23864,#23865,#23866,#23867),.UNSPECIFIED.,.F.,.F.)
B_SPLINE_CURVE_WITH_KNOTS((6,1,1,1,1,1,1,1,1,1,1,1,1,1,1,1,1,1,1,1,1,1,
1,1,1,1,1,1,1,1,1,1,1,1,1,1,1,1,1,1,1,1,1,1,1,1,1,1,1,1,1,1,1,1,1,1,1,1,
1,1,1,1,1,1,1,6),(0.,0.0153846153846154,0.0307692307692308,0.0461538461538462,
0.0615384615384615,0.0769230769230769,0.0923076923076923,0.107692307692308,
0.123076923076923,0.138461538461538,0.153846153846154,0.169230769230769,
0.184615384615385,0.2,0.215384615384615,0.230769230769231,0.246153846153846,
0.261538461538462,0.276923076923077,0.292307692307692,0.307692307692308,
0.323076923076923,0.338461538461538,0.353846153846154,0.369230769230769,
0.384615384615385,0.4,0.415384615384615,0.430769230769231,0.446153846153846,
0.461538461538462,0.476923076923077,0.492307692307692,0.507692307692308,
0.523076923076923,0.538461538461538,0.553846153846154,0.569230769230769,
0.584615384615384,0.6,0.615384615384615,0.63076923076923,0.646153846153846,
0.661538461538461,0.676923076923076,0.692307692307692,0.707692307692307,
0.723076923076922,0.738461538461538,0.753846153846153,0.769230769230768,
0.784615384615384,0.799999999999999,0.815384615384614,0.83076923076923,
0.846153846153845,0.86153846153846,0.876923076923076,0.892307692307691,
0.907692307692306,0.923076923076922,0.938461538461537,0.953846153846152,
0.969230769230768,0.984615384615383,1.),.UNSPECIFIED.)
CURVE()
GEOMETRIC_REPRESENTATION_ITEM()
RATIONAL_B_SPLINE_CURVE((1.,1.,1.,1.,1.,1.,1.,1.,1.,1.,1.,1.,1.,1.,1.,1.,
1.,1.,1.,1.,1.,1.,1.,1.,1.,1.,1.,1.,1.,1.,1.,1.,1.,1.,1.,1.,1.,1.,1.,1.,
1.,1.,1.,1.,1.,1.,1.,1.,1.,1.,1.,1.,1.,1.,1.,1.,1.,1.,1.,1.,1.,1.,1.,1.,
1.,1.,1.,1.,1.,1.))
REPRESENTATION_ITEM('')
);
#85=(
BOUNDED_CURVE()
B_SPLINE_CURVE(5,(#23871,#23872,#23873,#23874,#23875,#23876,#23877,#23878,
#23879,#23880,#23881,#23882,#23883,#23884,#23885,#23886,#23887,#23888,#23889,
#23890,#23891,#23892,#23893,#23894,#23895,#23896,#23897,#23898,#23899,#23900,
#23901,#23902,#23903,#23904,#23905,#23906,#23907,#23908,#23909,#23910,#23911,
#23912,#23913,#23914,#23915,#23916,#23917,#23918,#23919,#23920,#23921,#23922,
#23923,#23924,#23925,#23926,#23927,#23928,#23929,#23930,#23931,#23932,#23933,
#23934,#23935,#23936,#23937,#23938,#23939,#23940),.UNSPECIFIED.,.F.,.F.)
B_SPLINE_CURVE_WITH_KNOTS((6,1,1,1,1,1,1,1,1,1,1,1,1,1,1,1,1,1,1,1,1,1,
1,1,1,1,1,1,1,1,1,1,1,1,1,1,1,1,1,1,1,1,1,1,1,1,1,1,1,1,1,1,1,1,1,1,1,1,
1,1,1,1,1,1,1,6),(0.,0.0153846153846154,0.0307692307692308,0.0461538461538462,
0.0615384615384615,0.0769230769230769,0.0923076923076923,0.107692307692308,
0.123076923076923,0.138461538461538,0.153846153846154,0.169230769230769,
0.184615384615385,0.2,0.215384615384615,0.230769230769231,0.246153846153846,
0.261538461538462,0.276923076923077,0.292307692307692,0.307692307692308,
0.323076923076923,0.338461538461538,0.353846153846154,0.369230769230769,
0.384615384615385,0.4,0.415384615384615,0.430769230769231,0.446153846153846,
0.461538461538462,0.476923076923077,0.492307692307692,0.507692307692308,
0.523076923076923,0.538461538461538,0.553846153846154,0.569230769230769,
0.584615384615384,0.6,0.615384615384615,0.63076923076923,0.646153846153846,
0.661538461538461,0.676923076923076,0.692307692307692,0.707692307692307,
0.723076923076922,0.738461538461538,0.753846153846153,0.769230769230768,
0.784615384615384,0.799999999999999,0.815384615384614,0.83076923076923,
0.846153846153845,0.86153846153846,0.876923076923076,0.892307692307691,
0.907692307692306,0.923076923076922,0.938461538461537,0.953846153846152,
0.969230769230768,0.984615384615383,1.),.UNSPECIFIED.)
CURVE()
GEOMETRIC_REPRESENTATION_ITEM()
RATIONAL_B_SPLINE_CURVE((1.,1.,1.,1.,1.,1.,1.,1.,1.,1.,1.,1.,1.,1.,1.,1.,
1.,1.,1.,1.,1.,1.,1.,1.,1.,1.,1.,1.,1.,1.,1.,1.,1.,1.,1.,1.,1.,1.,1.,1.,
1.,1.,1.,1.,1.,1.,1.,1.,1.,1.,1.,1.,1.,1.,1.,1.,1.,1.,1.,1.,1.,1.,1.,1.,
1.,1.,1.,1.,1.,1.))
REPRESENTATION_ITEM('')
);
#86=(
BOUNDED_CURVE()
B_SPLINE_CURVE(5,(#23944,#23945,#23946,#23947,#23948,#23949,#23950,#23951,
#23952,#23953,#23954,#23955,#23956,#23957,#23958,#23959,#23960,#23961,#23962,
#23963,#23964,#23965,#23966,#23967,#23968,#23969,#23970,#23971,#23972,#23973,
#23974,#23975,#23976,#23977,#23978,#23979,#23980,#23981,#23982,#23983,#23984,
#23985,#23986,#23987,#23988,#23989,#23990,#23991,#23992,#23993,#23994,#23995,
#23996,#23997,#23998,#23999,#24000,#24001,#24002,#24003,#24004,#24005,#24006,
#24007,#24008,#24009,#24010,#24011,#24012,#24013),.UNSPECIFIED.,.F.,.F.)
B_SPLINE_CURVE_WITH_KNOTS((6,1,1,1,1,1,1,1,1,1,1,1,1,1,1,1,1,1,1,1,1,1,
1,1,1,1,1,1,1,1,1,1,1,1,1,1,1,1,1,1,1,1,1,1,1,1,1,1,1,1,1,1,1,1,1,1,1,1,
1,1,1,1,1,1,1,6),(0.,0.0153846153846154,0.0307692307692308,0.0461538461538462,
0.0615384615384615,0.0769230769230769,0.0923076923076923,0.107692307692308,
0.123076923076923,0.138461538461538,0.153846153846154,0.169230769230769,
0.184615384615385,0.2,0.215384615384615,0.230769230769231,0.246153846153846,
0.261538461538462,0.276923076923077,0.292307692307692,0.307692307692308,
0.323076923076923,0.338461538461538,0.353846153846154,0.369230769230769,
0.384615384615385,0.4,0.415384615384615,0.430769230769231,0.446153846153846,
0.461538461538462,0.476923076923077,0.492307692307692,0.507692307692308,
0.523076923076923,0.538461538461538,0.553846153846154,0.569230769230769,
0.584615384615384,0.6,0.615384615384615,0.63076923076923,0.646153846153846,
0.661538461538461,0.676923076923076,0.692307692307692,0.707692307692307,
0.723076923076922,0.738461538461538,0.753846153846153,0.769230769230768,
0.784615384615384,0.799999999999999,0.815384615384614,0.83076923076923,
0.846153846153845,0.86153846153846,0.876923076923076,0.892307692307691,
0.907692307692306,0.923076923076922,0.938461538461537,0.953846153846152,
0.969230769230768,0.984615384615383,1.),.UNSPECIFIED.)
CURVE()
GEOMETRIC_REPRESENTATION_ITEM()
RATIONAL_B_SPLINE_CURVE((1.,1.,1.,1.,1.,1.,1.,1.,1.,1.,1.,1.,1.,1.,1.,1.,
1.,1.,1.,1.,1.,1.,1.,1.,1.,1.,1.,1.,1.,1.,1.,1.,1.,1.,1.,1.,1.,1.,1.,1.,
1.,1.,1.,1.,1.,1.,1.,1.,1.,1.,1.,1.,1.,1.,1.,1.,1.,1.,1.,1.,1.,1.,1.,1.,
1.,1.,1.,1.,1.,1.))
REPRESENTATION_ITEM('')
);
#87=(
BOUNDED_CURVE()
B_SPLINE_CURVE(5,(#24017,#24018,#24019,#24020,#24021,#24022,#24023,#24024,
#24025,#24026,#24027,#24028,#24029,#24030,#24031,#24032,#24033,#24034,#24035,
#24036,#24037,#24038,#24039,#24040,#24041,#24042,#24043,#24044,#24045,#24046,
#24047,#24048,#24049,#24050,#24051,#24052,#24053,#24054,#24055,#24056,#24057,
#24058,#24059,#24060,#24061,#24062,#24063,#24064,#24065,#24066,#24067,#24068,
#24069,#24070,#24071,#24072,#24073,#24074,#24075,#24076,#24077,#24078,#24079,
#24080,#24081,#24082,#24083,#24084,#24085,#24086),.UNSPECIFIED.,.F.,.F.)
B_SPLINE_CURVE_WITH_KNOTS((6,1,1,1,1,1,1,1,1,1,1,1,1,1,1,1,1,1,1,1,1,1,
1,1,1,1,1,1,1,1,1,1,1,1,1,1,1,1,1,1,1,1,1,1,1,1,1,1,1,1,1,1,1,1,1,1,1,1,
1,1,1,1,1,1,1,6),(0.,0.0153846153846154,0.0307692307692308,0.0461538461538462,
0.0615384615384615,0.0769230769230769,0.0923076923076923,0.107692307692308,
0.123076923076923,0.138461538461538,0.153846153846154,0.169230769230769,
0.184615384615385,0.2,0.215384615384615,0.230769230769231,0.246153846153846,
0.261538461538462,0.276923076923077,0.292307692307692,0.307692307692308,
0.323076923076923,0.338461538461538,0.353846153846154,0.369230769230769,
0.384615384615385,0.4,0.415384615384615,0.430769230769231,0.446153846153846,
0.461538461538462,0.476923076923077,0.492307692307692,0.507692307692308,
0.523076923076923,0.538461538461538,0.553846153846154,0.569230769230769,
0.584615384615384,0.6,0.615384615384615,0.63076923076923,0.646153846153846,
0.661538461538461,0.676923076923076,0.692307692307692,0.707692307692307,
0.723076923076922,0.738461538461538,0.753846153846153,0.769230769230768,
0.784615384615384,0.799999999999999,0.815384615384614,0.83076923076923,
0.846153846153845,0.86153846153846,0.876923076923076,0.892307692307691,
0.907692307692306,0.923076923076922,0.938461538461537,0.953846153846152,
0.969230769230768,0.984615384615383,1.),.UNSPECIFIED.)
CURVE()
GEOMETRIC_REPRESENTATION_ITEM()
RATIONAL_B_SPLINE_CURVE((1.,1.,1.,1.,1.,1.,1.,1.,1.,1.,1.,1.,1.,1.,1.,1.,
1.,1.,1.,1.,1.,1.,1.,1.,1.,1.,1.,1.,1.,1.,1.,1.,1.,1.,1.,1.,1.,1.,1.,1.,
1.,1.,1.,1.,1.,1.,1.,1.,1.,1.,1.,1.,1.,1.,1.,1.,1.,1.,1.,1.,1.,1.,1.,1.,
1.,1.,1.,1.,1.,1.))
REPRESENTATION_ITEM('')
);
#88=(
BOUNDED_CURVE()
B_SPLINE_CURVE(5,(#24090,#24091,#24092,#24093,#24094,#24095,#24096,#24097,
#24098,#24099,#24100,#24101,#24102,#24103,#24104,#24105,#24106,#24107,#24108,
#24109,#24110,#24111,#24112,#24113,#24114,#24115,#24116,#24117,#24118,#24119,
#24120,#24121,#24122,#24123,#24124,#24125,#24126,#24127,#24128,#24129,#24130,
#24131,#24132,#24133,#24134,#24135,#24136,#24137,#24138,#24139,#24140,#24141,
#24142,#24143,#24144,#24145,#24146,#24147,#24148,#24149,#24150,#24151,#24152,
#24153,#24154,#24155,#24156,#24157,#24158,#24159),.UNSPECIFIED.,.F.,.F.)
B_SPLINE_CURVE_WITH_KNOTS((6,1,1,1,1,1,1,1,1,1,1,1,1,1,1,1,1,1,1,1,1,1,
1,1,1,1,1,1,1,1,1,1,1,1,1,1,1,1,1,1,1,1,1,1,1,1,1,1,1,1,1,1,1,1,1,1,1,1,
1,1,1,1,1,1,1,6),(0.,0.0153846153846154,0.0307692307692308,0.0461538461538462,
0.0615384615384615,0.0769230769230769,0.0923076923076923,0.107692307692308,
0.123076923076923,0.138461538461538,0.153846153846154,0.169230769230769,
0.184615384615385,0.2,0.215384615384615,0.230769230769231,0.246153846153846,
0.261538461538462,0.276923076923077,0.292307692307692,0.307692307692308,
0.323076923076923,0.338461538461538,0.353846153846154,0.369230769230769,
0.384615384615385,0.4,0.415384615384615,0.430769230769231,0.446153846153846,
0.461538461538462,0.476923076923077,0.492307692307692,0.507692307692308,
0.523076923076923,0.538461538461538,0.553846153846154,0.569230769230769,
0.584615384615384,0.6,0.615384615384615,0.63076923076923,0.646153846153846,
0.661538461538461,0.676923076923076,0.692307692307692,0.707692307692307,
0.723076923076922,0.738461538461538,0.753846153846153,0.769230769230768,
0.784615384615384,0.799999999999999,0.815384615384614,0.83076923076923,
0.846153846153845,0.86153846153846,0.876923076923076,0.892307692307691,
0.907692307692306,0.923076923076922,0.938461538461537,0.953846153846152,
0.969230769230768,0.984615384615383,1.),.UNSPECIFIED.)
CURVE()
GEOMETRIC_REPRESENTATION_ITEM()
RATIONAL_B_SPLINE_CURVE((1.,1.,1.,1.,1.,1.,1.,1.,1.,1.,1.,1.,1.,1.,1.,1.,
1.,1.,1.,1.,1.,1.,1.,1.,1.,1.,1.,1.,1.,1.,1.,1.,1.,1.,1.,1.,1.,1.,1.,1.,
1.,1.,1.,1.,1.,1.,1.,1.,1.,1.,1.,1.,1.,1.,1.,1.,1.,1.,1.,1.,1.,1.,1.,1.,
1.,1.,1.,1.,1.,1.))
REPRESENTATION_ITEM('')
);
#89=(
BOUNDED_CURVE()
B_SPLINE_CURVE(5,(#24163,#24164,#24165,#24166,#24167,#24168,#24169,#24170,
#24171,#24172,#24173,#24174,#24175,#24176,#24177,#24178,#24179,#24180,#24181,
#24182,#24183,#24184,#24185,#24186,#24187,#24188,#24189,#24190,#24191,#24192,
#24193,#24194,#24195,#24196,#24197,#24198,#24199,#24200,#24201,#24202,#24203,
#24204,#24205,#24206,#24207,#24208,#24209,#24210,#24211,#24212,#24213,#24214,
#24215,#24216,#24217,#24218,#24219,#24220,#24221,#24222,#24223,#24224,#24225,
#24226,#24227,#24228,#24229,#24230,#24231,#24232),.UNSPECIFIED.,.F.,.F.)
B_SPLINE_CURVE_WITH_KNOTS((6,1,1,1,1,1,1,1,1,1,1,1,1,1,1,1,1,1,1,1,1,1,
1,1,1,1,1,1,1,1,1,1,1,1,1,1,1,1,1,1,1,1,1,1,1,1,1,1,1,1,1,1,1,1,1,1,1,1,
1,1,1,1,1,1,1,6),(0.,0.0153846153846154,0.0307692307692308,0.0461538461538462,
0.0615384615384615,0.0769230769230769,0.0923076923076923,0.107692307692308,
0.123076923076923,0.138461538461538,0.153846153846154,0.169230769230769,
0.184615384615385,0.2,0.215384615384615,0.230769230769231,0.246153846153846,
0.261538461538462,0.276923076923077,0.292307692307692,0.307692307692308,
0.323076923076923,0.338461538461538,0.353846153846154,0.369230769230769,
0.384615384615385,0.4,0.415384615384615,0.430769230769231,0.446153846153846,
0.461538461538462,0.476923076923077,0.492307692307692,0.507692307692308,
0.523076923076923,0.538461538461538,0.553846153846154,0.569230769230769,
0.584615384615384,0.6,0.615384615384615,0.63076923076923,0.646153846153846,
0.661538461538461,0.676923076923076,0.692307692307692,0.707692307692307,
0.723076923076922,0.738461538461538,0.753846153846153,0.769230769230768,
0.784615384615384,0.799999999999999,0.815384615384614,0.83076923076923,
0.846153846153845,0.86153846153846,0.876923076923076,0.892307692307691,
0.907692307692306,0.923076923076922,0.938461538461537,0.953846153846152,
0.969230769230768,0.984615384615383,1.),.UNSPECIFIED.)
CURVE()
GEOMETRIC_REPRESENTATION_ITEM()
RATIONAL_B_SPLINE_CURVE((1.,1.,1.,1.,1.,1.,1.,1.,1.,1.,1.,1.,1.,1.,1.,1.,
1.,1.,1.,1.,1.,1.,1.,1.,1.,1.,1.,1.,1.,1.,1.,1.,1.,1.,1.,1.,1.,1.,1.,1.,
1.,1.,1.,1.,1.,1.,1.,1.,1.,1.,1.,1.,1.,1.,1.,1.,1.,1.,1.,1.,1.,1.,1.,1.,
1.,1.,1.,1.,1.,1.))
REPRESENTATION_ITEM('')
);
#90=(
BOUNDED_CURVE()
B_SPLINE_CURVE(5,(#24235,#24236,#24237,#24238,#24239,#24240,#24241,#24242,
#24243,#24244,#24245,#24246,#24247,#24248,#24249,#24250,#24251,#24252,#24253,
#24254,#24255,#24256,#24257,#24258,#24259,#24260,#24261,#24262,#24263,#24264,
#24265,#24266,#24267,#24268,#24269,#24270,#24271,#24272,#24273,#24274,#24275,
#24276,#24277,#24278,#24279,#24280,#24281,#24282,#24283,#24284,#24285,#24286,
#24287,#24288,#24289,#24290,#24291,#24292,#24293,#24294,#24295,#24296,#24297,
#24298,#24299,#24300,#24301,#24302,#24303,#24304),.UNSPECIFIED.,.F.,.F.)
B_SPLINE_CURVE_WITH_KNOTS((6,1,1,1,1,1,1,1,1,1,1,1,1,1,1,1,1,1,1,1,1,1,
1,1,1,1,1,1,1,1,1,1,1,1,1,1,1,1,1,1,1,1,1,1,1,1,1,1,1,1,1,1,1,1,1,1,1,1,
1,1,1,1,1,1,1,6),(0.,0.0153846153846154,0.0307692307692308,0.0461538461538462,
0.0615384615384615,0.0769230769230769,0.0923076923076923,0.107692307692308,
0.123076923076923,0.138461538461538,0.153846153846154,0.169230769230769,
0.184615384615385,0.2,0.215384615384615,0.230769230769231,0.246153846153846,
0.261538461538462,0.276923076923077,0.292307692307692,0.307692307692308,
0.323076923076923,0.338461538461538,0.353846153846154,0.369230769230769,
0.384615384615385,0.4,0.415384615384615,0.430769230769231,0.446153846153846,
0.461538461538462,0.476923076923077,0.492307692307692,0.507692307692308,
0.523076923076923,0.538461538461538,0.553846153846154,0.569230769230769,
0.584615384615384,0.6,0.615384615384615,0.63076923076923,0.646153846153846,
0.661538461538461,0.676923076923076,0.692307692307692,0.707692307692307,
0.723076923076922,0.738461538461538,0.753846153846153,0.769230769230768,
0.784615384615384,0.799999999999999,0.815384615384614,0.83076923076923,
0.846153846153845,0.86153846153846,0.876923076923076,0.892307692307691,
0.907692307692306,0.923076923076922,0.938461538461537,0.953846153846152,
0.969230769230768,0.984615384615383,1.),.UNSPECIFIED.)
CURVE()
GEOMETRIC_REPRESENTATION_ITEM()
RATIONAL_B_SPLINE_CURVE((1.,1.,1.,1.,1.,1.,1.,1.,1.,1.,1.,1.,1.,1.,1.,1.,
1.,1.,1.,1.,1.,1.,1.,1.,1.,1.,1.,1.,1.,1.,1.,1.,1.,1.,1.,1.,1.,1.,1.,1.,
1.,1.,1.,1.,1.,1.,1.,1.,1.,1.,1.,1.,1.,1.,1.,1.,1.,1.,1.,1.,1.,1.,1.,1.,
1.,1.,1.,1.,1.,1.))
REPRESENTATION_ITEM('')
);
#91=(
BOUNDED_CURVE()
B_SPLINE_CURVE(5,(#24458,#24459,#24460,#24461,#24462,#24463,#24464,#24465,
#24466,#24467,#24468,#24469,#24470,#24471,#24472,#24473,#24474,#24475,#24476,
#24477,#24478,#24479,#24480,#24481,#24482,#24483,#24484,#24485,#24486,#24487,
#24488,#24489,#24490,#24491,#24492,#24493,#24494,#24495,#24496,#24497,#24498,
#24499,#24500,#24501,#24502,#24503,#24504,#24505,#24506,#24507,#24508,#24509,
#24510,#24511,#24512,#24513,#24514,#24515,#24516,#24517,#24518,#24519,#24520,
#24521,#24522,#24523,#24524,#24525,#24526,#24527),.UNSPECIFIED.,.F.,.F.)
B_SPLINE_CURVE_WITH_KNOTS((6,1,1,1,1,1,1,1,1,1,1,1,1,1,1,1,1,1,1,1,1,1,
1,1,1,1,1,1,1,1,1,1,1,1,1,1,1,1,1,1,1,1,1,1,1,1,1,1,1,1,1,1,1,1,1,1,1,1,
1,1,1,1,1,1,1,6),(-1.,-0.984615384615383,-0.969230769230768,-0.953846153846152,
-0.938461538461537,-0.923076923076922,-0.907692307692306,-0.892307692307691,
-0.876923076923076,-0.86153846153846,-0.846153846153845,-0.83076923076923,
-0.815384615384614,-0.799999999999999,-0.784615384615384,-0.769230769230768,
-0.753846153846153,-0.738461538461538,-0.723076923076922,-0.707692307692307,
-0.692307692307692,-0.676923076923076,-0.661538461538461,-0.646153846153846,
-0.63076923076923,-0.615384615384615,-0.6,-0.584615384615384,-0.569230769230769,
-0.553846153846154,-0.538461538461538,-0.523076923076923,-0.507692307692308,
-0.492307692307692,-0.476923076923077,-0.461538461538462,-0.446153846153846,
-0.430769230769231,-0.415384615384615,-0.4,-0.384615384615385,-0.369230769230769,
-0.353846153846154,-0.338461538461538,-0.323076923076923,-0.307692307692308,
-0.292307692307692,-0.276923076923077,-0.261538461538462,-0.246153846153846,
-0.230769230769231,-0.215384615384615,-0.2,-0.184615384615385,-0.169230769230769,
-0.153846153846154,-0.138461538461538,-0.123076923076923,-0.107692307692308,
-0.0923076923076923,-0.0769230769230769,-0.0615384615384615,-0.0461538461538462,
-0.0307692307692308,-0.0153846153846154,0.),.UNSPECIFIED.)
CURVE()
GEOMETRIC_REPRESENTATION_ITEM()
RATIONAL_B_SPLINE_CURVE((1.,1.,1.,1.,1.,1.,1.,1.,1.,1.,1.,1.,1.,1.,1.,1.,
1.,1.,1.,1.,1.,1.,1.,1.,1.,1.,1.,1.,1.,1.,1.,1.,1.,1.,1.,1.,1.,1.,1.,1.,
1.,1.,1.,1.,1.,1.,1.,1.,1.,1.,1.,1.,1.,1.,1.,1.,1.,1.,1.,1.,1.,1.,1.,1.,
1.,1.,1.,1.,1.,1.))
REPRESENTATION_ITEM('')
);
#92=(
BOUNDED_CURVE()
B_SPLINE_CURVE(5,(#24674,#24675,#24676,#24677,#24678,#24679,#24680,#24681,
#24682,#24683,#24684,#24685,#24686,#24687,#24688,#24689,#24690,#24691,#24692,
#24693,#24694,#24695,#24696,#24697,#24698,#24699,#24700,#24701,#24702,#24703,
#24704,#24705,#24706,#24707,#24708,#24709,#24710,#24711,#24712,#24713,#24714,
#24715,#24716,#24717,#24718,#24719,#24720,#24721,#24722,#24723,#24724,#24725,
#24726,#24727,#24728,#24729,#24730,#24731,#24732,#24733,#24734,#24735,#24736,
#24737,#24738,#24739,#24740,#24741,#24742,#24743),.UNSPECIFIED.,.F.,.F.)
B_SPLINE_CURVE_WITH_KNOTS((6,1,1,1,1,1,1,1,1,1,1,1,1,1,1,1,1,1,1,1,1,1,
1,1,1,1,1,1,1,1,1,1,1,1,1,1,1,1,1,1,1,1,1,1,1,1,1,1,1,1,1,1,1,1,1,1,1,1,
1,1,1,1,1,1,1,6),(-1.,-0.984615384615383,-0.969230769230768,-0.953846153846152,
-0.938461538461537,-0.923076923076922,-0.907692307692306,-0.892307692307691,
-0.876923076923076,-0.86153846153846,-0.846153846153845,-0.83076923076923,
-0.815384615384614,-0.799999999999999,-0.784615384615384,-0.769230769230768,
-0.753846153846153,-0.738461538461538,-0.723076923076922,-0.707692307692307,
-0.692307692307692,-0.676923076923076,-0.661538461538461,-0.646153846153846,
-0.63076923076923,-0.615384615384615,-0.6,-0.584615384615384,-0.569230769230769,
-0.553846153846154,-0.538461538461538,-0.523076923076923,-0.507692307692308,
-0.492307692307692,-0.476923076923077,-0.461538461538462,-0.446153846153846,
-0.430769230769231,-0.415384615384615,-0.4,-0.384615384615385,-0.369230769230769,
-0.353846153846154,-0.338461538461538,-0.323076923076923,-0.307692307692308,
-0.292307692307692,-0.276923076923077,-0.261538461538462,-0.246153846153846,
-0.230769230769231,-0.215384615384615,-0.2,-0.184615384615385,-0.169230769230769,
-0.153846153846154,-0.138461538461538,-0.123076923076923,-0.107692307692308,
-0.0923076923076923,-0.0769230769230769,-0.0615384615384615,-0.0461538461538462,
-0.0307692307692308,-0.0153846153846154,0.),.UNSPECIFIED.)
CURVE()
GEOMETRIC_REPRESENTATION_ITEM()
RATIONAL_B_SPLINE_CURVE((1.,1.,1.,1.,1.,1.,1.,1.,1.,1.,1.,1.,1.,1.,1.,1.,
1.,1.,1.,1.,1.,1.,1.,1.,1.,1.,1.,1.,1.,1.,1.,1.,1.,1.,1.,1.,1.,1.,1.,1.,
1.,1.,1.,1.,1.,1.,1.,1.,1.,1.,1.,1.,1.,1.,1.,1.,1.,1.,1.,1.,1.,1.,1.,1.,
1.,1.,1.,1.,1.,1.))
REPRESENTATION_ITEM('')
);
#93=(
BOUNDED_CURVE()
B_SPLINE_CURVE(5,(#24890,#24891,#24892,#24893,#24894,#24895,#24896,#24897,
#24898,#24899,#24900,#24901,#24902,#24903,#24904,#24905,#24906,#24907,#24908,
#24909,#24910,#24911,#24912,#24913,#24914,#24915,#24916,#24917,#24918,#24919,
#24920,#24921,#24922,#24923,#24924,#24925,#24926,#24927,#24928,#24929,#24930,
#24931,#24932,#24933,#24934,#24935,#24936,#24937,#24938,#24939,#24940,#24941,
#24942,#24943,#24944,#24945,#24946,#24947,#24948,#24949,#24950,#24951,#24952,
#24953,#24954,#24955,#24956,#24957,#24958,#24959),.UNSPECIFIED.,.F.,.F.)
B_SPLINE_CURVE_WITH_KNOTS((6,1,1,1,1,1,1,1,1,1,1,1,1,1,1,1,1,1,1,1,1,1,
1,1,1,1,1,1,1,1,1,1,1,1,1,1,1,1,1,1,1,1,1,1,1,1,1,1,1,1,1,1,1,1,1,1,1,1,
1,1,1,1,1,1,1,6),(-1.,-0.984615384615383,-0.969230769230768,-0.953846153846152,
-0.938461538461537,-0.923076923076922,-0.907692307692306,-0.892307692307691,
-0.876923076923076,-0.86153846153846,-0.846153846153845,-0.83076923076923,
-0.815384615384614,-0.799999999999999,-0.784615384615384,-0.769230769230768,
-0.753846153846153,-0.738461538461538,-0.723076923076922,-0.707692307692307,
-0.692307692307692,-0.676923076923076,-0.661538461538461,-0.646153846153846,
-0.63076923076923,-0.615384615384615,-0.6,-0.584615384615384,-0.569230769230769,
-0.553846153846154,-0.538461538461538,-0.523076923076923,-0.507692307692308,
-0.492307692307692,-0.476923076923077,-0.461538461538462,-0.446153846153846,
-0.430769230769231,-0.415384615384615,-0.4,-0.384615384615385,-0.369230769230769,
-0.353846153846154,-0.338461538461538,-0.323076923076923,-0.307692307692308,
-0.292307692307692,-0.276923076923077,-0.261538461538462,-0.246153846153846,
-0.230769230769231,-0.215384615384615,-0.2,-0.184615384615385,-0.169230769230769,
-0.153846153846154,-0.138461538461538,-0.123076923076923,-0.107692307692308,
-0.0923076923076923,-0.0769230769230769,-0.0615384615384615,-0.0461538461538462,
-0.0307692307692308,-0.0153846153846154,0.),.UNSPECIFIED.)
CURVE()
GEOMETRIC_REPRESENTATION_ITEM()
RATIONAL_B_SPLINE_CURVE((1.,1.,1.,1.,1.,1.,1.,1.,1.,1.,1.,1.,1.,1.,1.,1.,
1.,1.,1.,1.,1.,1.,1.,1.,1.,1.,1.,1.,1.,1.,1.,1.,1.,1.,1.,1.,1.,1.,1.,1.,
1.,1.,1.,1.,1.,1.,1.,1.,1.,1.,1.,1.,1.,1.,1.,1.,1.,1.,1.,1.,1.,1.,1.,1.,
1.,1.,1.,1.,1.,1.))
REPRESENTATION_ITEM('')
);
#94=(
BOUNDED_CURVE()
B_SPLINE_CURVE(5,(#25106,#25107,#25108,#25109,#25110,#25111,#25112,#25113,
#25114,#25115,#25116,#25117,#25118,#25119,#25120,#25121,#25122,#25123,#25124,
#25125,#25126,#25127,#25128,#25129,#25130,#25131,#25132,#25133,#25134,#25135,
#25136,#25137,#25138,#25139,#25140,#25141,#25142,#25143,#25144,#25145,#25146,
#25147,#25148,#25149,#25150,#25151,#25152,#25153,#25154,#25155,#25156,#25157,
#25158,#25159,#25160,#25161,#25162,#25163,#25164,#25165,#25166,#25167,#25168,
#25169,#25170,#25171,#25172,#25173,#25174,#25175),.UNSPECIFIED.,.F.,.F.)
B_SPLINE_CURVE_WITH_KNOTS((6,1,1,1,1,1,1,1,1,1,1,1,1,1,1,1,1,1,1,1,1,1,
1,1,1,1,1,1,1,1,1,1,1,1,1,1,1,1,1,1,1,1,1,1,1,1,1,1,1,1,1,1,1,1,1,1,1,1,
1,1,1,1,1,1,1,6),(-1.,-0.984615384615383,-0.969230769230768,-0.953846153846152,
-0.938461538461537,-0.923076923076922,-0.907692307692306,-0.892307692307691,
-0.876923076923076,-0.86153846153846,-0.846153846153845,-0.83076923076923,
-0.815384615384614,-0.799999999999999,-0.784615384615384,-0.769230769230768,
-0.753846153846153,-0.738461538461538,-0.723076923076922,-0.707692307692307,
-0.692307692307692,-0.676923076923076,-0.661538461538461,-0.646153846153846,
-0.63076923076923,-0.615384615384615,-0.6,-0.584615384615384,-0.569230769230769,
-0.553846153846154,-0.538461538461538,-0.523076923076923,-0.507692307692308,
-0.492307692307692,-0.476923076923077,-0.461538461538462,-0.446153846153846,
-0.430769230769231,-0.415384615384615,-0.4,-0.384615384615385,-0.369230769230769,
-0.353846153846154,-0.338461538461538,-0.323076923076923,-0.307692307692308,
-0.292307692307692,-0.276923076923077,-0.261538461538462,-0.246153846153846,
-0.230769230769231,-0.215384615384615,-0.2,-0.184615384615385,-0.169230769230769,
-0.153846153846154,-0.138461538461538,-0.123076923076923,-0.107692307692308,
-0.0923076923076923,-0.0769230769230769,-0.0615384615384615,-0.0461538461538462,
-0.0307692307692308,-0.0153846153846154,0.),.UNSPECIFIED.)
CURVE()
GEOMETRIC_REPRESENTATION_ITEM()
RATIONAL_B_SPLINE_CURVE((1.,1.,1.,1.,1.,1.,1.,1.,1.,1.,1.,1.,1.,1.,1.,1.,
1.,1.,1.,1.,1.,1.,1.,1.,1.,1.,1.,1.,1.,1.,1.,1.,1.,1.,1.,1.,1.,1.,1.,1.,
1.,1.,1.,1.,1.,1.,1.,1.,1.,1.,1.,1.,1.,1.,1.,1.,1.,1.,1.,1.,1.,1.,1.,1.,
1.,1.,1.,1.,1.,1.))
REPRESENTATION_ITEM('')
);
#95=(
BOUNDED_CURVE()
B_SPLINE_CURVE(5,(#25322,#25323,#25324,#25325,#25326,#25327,#25328,#25329,
#25330,#25331,#25332,#25333,#25334,#25335,#25336,#25337,#25338,#25339,#25340,
#25341,#25342,#25343,#25344,#25345,#25346,#25347,#25348,#25349,#25350,#25351,
#25352,#25353,#25354,#25355,#25356,#25357,#25358,#25359,#25360,#25361,#25362,
#25363,#25364,#25365,#25366,#25367,#25368,#25369,#25370,#25371,#25372,#25373,
#25374,#25375,#25376,#25377,#25378,#25379,#25380,#25381,#25382,#25383,#25384,
#25385,#25386,#25387,#25388,#25389,#25390,#25391),.UNSPECIFIED.,.F.,.F.)
B_SPLINE_CURVE_WITH_KNOTS((6,1,1,1,1,1,1,1,1,1,1,1,1,1,1,1,1,1,1,1,1,1,
1,1,1,1,1,1,1,1,1,1,1,1,1,1,1,1,1,1,1,1,1,1,1,1,1,1,1,1,1,1,1,1,1,1,1,1,
1,1,1,1,1,1,1,6),(-1.,-0.984615384615383,-0.969230769230768,-0.953846153846152,
-0.938461538461537,-0.923076923076922,-0.907692307692306,-0.892307692307691,
-0.876923076923076,-0.86153846153846,-0.846153846153845,-0.83076923076923,
-0.815384615384614,-0.799999999999999,-0.784615384615384,-0.769230769230768,
-0.753846153846153,-0.738461538461538,-0.723076923076922,-0.707692307692307,
-0.692307692307692,-0.676923076923076,-0.661538461538461,-0.646153846153846,
-0.63076923076923,-0.615384615384615,-0.6,-0.584615384615384,-0.569230769230769,
-0.553846153846154,-0.538461538461538,-0.523076923076923,-0.507692307692308,
-0.492307692307692,-0.476923076923077,-0.461538461538462,-0.446153846153846,
-0.430769230769231,-0.415384615384615,-0.4,-0.384615384615385,-0.369230769230769,
-0.353846153846154,-0.338461538461538,-0.323076923076923,-0.307692307692308,
-0.292307692307692,-0.276923076923077,-0.261538461538462,-0.246153846153846,
-0.230769230769231,-0.215384615384615,-0.2,-0.184615384615385,-0.169230769230769,
-0.153846153846154,-0.138461538461538,-0.123076923076923,-0.107692307692308,
-0.0923076923076923,-0.0769230769230769,-0.0615384615384615,-0.0461538461538462,
-0.0307692307692308,-0.0153846153846154,0.),.UNSPECIFIED.)
CURVE()
GEOMETRIC_REPRESENTATION_ITEM()
RATIONAL_B_SPLINE_CURVE((1.,1.,1.,1.,1.,1.,1.,1.,1.,1.,1.,1.,1.,1.,1.,1.,
1.,1.,1.,1.,1.,1.,1.,1.,1.,1.,1.,1.,1.,1.,1.,1.,1.,1.,1.,1.,1.,1.,1.,1.,
1.,1.,1.,1.,1.,1.,1.,1.,1.,1.,1.,1.,1.,1.,1.,1.,1.,1.,1.,1.,1.,1.,1.,1.,
1.,1.,1.,1.,1.,1.))
REPRESENTATION_ITEM('')
);
#96=(
BOUNDED_CURVE()
B_SPLINE_CURVE(5,(#25538,#25539,#25540,#25541,#25542,#25543,#25544,#25545,
#25546,#25547,#25548,#25549,#25550,#25551,#25552,#25553,#25554,#25555,#25556,
#25557,#25558,#25559,#25560,#25561,#25562,#25563,#25564,#25565,#25566,#25567,
#25568,#25569,#25570,#25571,#25572,#25573,#25574,#25575,#25576,#25577,#25578,
#25579,#25580,#25581,#25582,#25583,#25584,#25585,#25586,#25587,#25588,#25589,
#25590,#25591,#25592,#25593,#25594,#25595,#25596,#25597,#25598,#25599,#25600,
#25601,#25602,#25603,#25604,#25605,#25606,#25607),.UNSPECIFIED.,.F.,.F.)
B_SPLINE_CURVE_WITH_KNOTS((6,1,1,1,1,1,1,1,1,1,1,1,1,1,1,1,1,1,1,1,1,1,
1,1,1,1,1,1,1,1,1,1,1,1,1,1,1,1,1,1,1,1,1,1,1,1,1,1,1,1,1,1,1,1,1,1,1,1,
1,1,1,1,1,1,1,6),(-1.,-0.984615384615383,-0.969230769230768,-0.953846153846152,
-0.938461538461537,-0.923076923076922,-0.907692307692306,-0.892307692307691,
-0.876923076923076,-0.86153846153846,-0.846153846153845,-0.83076923076923,
-0.815384615384614,-0.799999999999999,-0.784615384615384,-0.769230769230768,
-0.753846153846153,-0.738461538461538,-0.723076923076922,-0.707692307692307,
-0.692307692307692,-0.676923076923076,-0.661538461538461,-0.646153846153846,
-0.63076923076923,-0.615384615384615,-0.6,-0.584615384615384,-0.569230769230769,
-0.553846153846154,-0.538461538461538,-0.523076923076923,-0.507692307692308,
-0.492307692307692,-0.476923076923077,-0.461538461538462,-0.446153846153846,
-0.430769230769231,-0.415384615384615,-0.4,-0.384615384615385,-0.369230769230769,
-0.353846153846154,-0.338461538461538,-0.323076923076923,-0.307692307692308,
-0.292307692307692,-0.276923076923077,-0.261538461538462,-0.246153846153846,
-0.230769230769231,-0.215384615384615,-0.2,-0.184615384615385,-0.169230769230769,
-0.153846153846154,-0.138461538461538,-0.123076923076923,-0.107692307692308,
-0.0923076923076923,-0.0769230769230769,-0.0615384615384615,-0.0461538461538462,
-0.0307692307692308,-0.0153846153846154,0.),.UNSPECIFIED.)
CURVE()
GEOMETRIC_REPRESENTATION_ITEM()
RATIONAL_B_SPLINE_CURVE((1.,1.,1.,1.,1.,1.,1.,1.,1.,1.,1.,1.,1.,1.,1.,1.,
1.,1.,1.,1.,1.,1.,1.,1.,1.,1.,1.,1.,1.,1.,1.,1.,1.,1.,1.,1.,1.,1.,1.,1.,
1.,1.,1.,1.,1.,1.,1.,1.,1.,1.,1.,1.,1.,1.,1.,1.,1.,1.,1.,1.,1.,1.,1.,1.,
1.,1.,1.,1.,1.,1.))
REPRESENTATION_ITEM('')
);
#97=(
BOUNDED_CURVE()
B_SPLINE_CURVE(5,(#25754,#25755,#25756,#25757,#25758,#25759,#25760,#25761,
#25762,#25763,#25764,#25765,#25766,#25767,#25768,#25769,#25770,#25771,#25772,
#25773,#25774,#25775,#25776,#25777,#25778,#25779,#25780,#25781,#25782,#25783,
#25784,#25785,#25786,#25787,#25788,#25789,#25790,#25791,#25792,#25793,#25794,
#25795,#25796,#25797,#25798,#25799,#25800,#25801,#25802,#25803,#25804,#25805,
#25806,#25807,#25808,#25809,#25810,#25811,#25812,#25813,#25814,#25815,#25816,
#25817,#25818,#25819,#25820,#25821,#25822,#25823),.UNSPECIFIED.,.F.,.F.)
B_SPLINE_CURVE_WITH_KNOTS((6,1,1,1,1,1,1,1,1,1,1,1,1,1,1,1,1,1,1,1,1,1,
1,1,1,1,1,1,1,1,1,1,1,1,1,1,1,1,1,1,1,1,1,1,1,1,1,1,1,1,1,1,1,1,1,1,1,1,
1,1,1,1,1,1,1,6),(-1.,-0.984615384615383,-0.969230769230768,-0.953846153846152,
-0.938461538461537,-0.923076923076922,-0.907692307692306,-0.892307692307691,
-0.876923076923076,-0.86153846153846,-0.846153846153845,-0.83076923076923,
-0.815384615384614,-0.799999999999999,-0.784615384615384,-0.769230769230768,
-0.753846153846153,-0.738461538461538,-0.723076923076922,-0.707692307692307,
-0.692307692307692,-0.676923076923076,-0.661538461538461,-0.646153846153846,
-0.63076923076923,-0.615384615384615,-0.6,-0.584615384615384,-0.569230769230769,
-0.553846153846154,-0.538461538461538,-0.523076923076923,-0.507692307692308,
-0.492307692307692,-0.476923076923077,-0.461538461538462,-0.446153846153846,
-0.430769230769231,-0.415384615384615,-0.4,-0.384615384615385,-0.369230769230769,
-0.353846153846154,-0.338461538461538,-0.323076923076923,-0.307692307692308,
-0.292307692307692,-0.276923076923077,-0.261538461538462,-0.246153846153846,
-0.230769230769231,-0.215384615384615,-0.2,-0.184615384615385,-0.169230769230769,
-0.153846153846154,-0.138461538461538,-0.123076923076923,-0.107692307692308,
-0.0923076923076923,-0.0769230769230769,-0.0615384615384615,-0.0461538461538462,
-0.0307692307692308,-0.0153846153846154,0.),.UNSPECIFIED.)
CURVE()
GEOMETRIC_REPRESENTATION_ITEM()
RATIONAL_B_SPLINE_CURVE((1.,1.,1.,1.,1.,1.,1.,1.,1.,1.,1.,1.,1.,1.,1.,1.,
1.,1.,1.,1.,1.,1.,1.,1.,1.,1.,1.,1.,1.,1.,1.,1.,1.,1.,1.,1.,1.,1.,1.,1.,
1.,1.,1.,1.,1.,1.,1.,1.,1.,1.,1.,1.,1.,1.,1.,1.,1.,1.,1.,1.,1.,1.,1.,1.,
1.,1.,1.,1.,1.,1.))
REPRESENTATION_ITEM('')
);
#98=(
BOUNDED_CURVE()
B_SPLINE_CURVE(5,(#25970,#25971,#25972,#25973,#25974,#25975,#25976,#25977,
#25978,#25979,#25980,#25981,#25982,#25983,#25984,#25985,#25986,#25987,#25988,
#25989,#25990,#25991,#25992,#25993,#25994,#25995,#25996,#25997,#25998,#25999,
#26000,#26001,#26002,#26003,#26004,#26005,#26006,#26007,#26008,#26009,#26010,
#26011,#26012,#26013,#26014,#26015,#26016,#26017,#26018,#26019,#26020,#26021,
#26022,#26023,#26024,#26025,#26026,#26027,#26028,#26029,#26030,#26031,#26032,
#26033,#26034,#26035,#26036,#26037,#26038,#26039),.UNSPECIFIED.,.F.,.F.)
B_SPLINE_CURVE_WITH_KNOTS((6,1,1,1,1,1,1,1,1,1,1,1,1,1,1,1,1,1,1,1,1,1,
1,1,1,1,1,1,1,1,1,1,1,1,1,1,1,1,1,1,1,1,1,1,1,1,1,1,1,1,1,1,1,1,1,1,1,1,
1,1,1,1,1,1,1,6),(-1.,-0.984615384615383,-0.969230769230768,-0.953846153846152,
-0.938461538461537,-0.923076923076922,-0.907692307692306,-0.892307692307691,
-0.876923076923076,-0.86153846153846,-0.846153846153845,-0.83076923076923,
-0.815384615384614,-0.799999999999999,-0.784615384615384,-0.769230769230768,
-0.753846153846153,-0.738461538461538,-0.723076923076922,-0.707692307692307,
-0.692307692307692,-0.676923076923076,-0.661538461538461,-0.646153846153846,
-0.63076923076923,-0.615384615384615,-0.6,-0.584615384615384,-0.569230769230769,
-0.553846153846154,-0.538461538461538,-0.523076923076923,-0.507692307692308,
-0.492307692307692,-0.476923076923077,-0.461538461538462,-0.446153846153846,
-0.430769230769231,-0.415384615384615,-0.4,-0.384615384615385,-0.369230769230769,
-0.353846153846154,-0.338461538461538,-0.323076923076923,-0.307692307692308,
-0.292307692307692,-0.276923076923077,-0.261538461538462,-0.246153846153846,
-0.230769230769231,-0.215384615384615,-0.2,-0.184615384615385,-0.169230769230769,
-0.153846153846154,-0.138461538461538,-0.123076923076923,-0.107692307692308,
-0.0923076923076923,-0.0769230769230769,-0.0615384615384615,-0.0461538461538462,
-0.0307692307692308,-0.0153846153846154,0.),.UNSPECIFIED.)
CURVE()
GEOMETRIC_REPRESENTATION_ITEM()
RATIONAL_B_SPLINE_CURVE((1.,1.,1.,1.,1.,1.,1.,1.,1.,1.,1.,1.,1.,1.,1.,1.,
1.,1.,1.,1.,1.,1.,1.,1.,1.,1.,1.,1.,1.,1.,1.,1.,1.,1.,1.,1.,1.,1.,1.,1.,
1.,1.,1.,1.,1.,1.,1.,1.,1.,1.,1.,1.,1.,1.,1.,1.,1.,1.,1.,1.,1.,1.,1.,1.,
1.,1.,1.,1.,1.,1.))
REPRESENTATION_ITEM('')
);
#99=(
BOUNDED_CURVE()
B_SPLINE_CURVE(5,(#26186,#26187,#26188,#26189,#26190,#26191,#26192,#26193,
#26194,#26195,#26196,#26197,#26198,#26199,#26200,#26201,#26202,#26203,#26204,
#26205,#26206,#26207,#26208,#26209,#26210,#26211,#26212,#26213,#26214,#26215,
#26216,#26217,#26218,#26219,#26220,#26221,#26222,#26223,#26224,#26225,#26226,
#26227,#26228,#26229,#26230,#26231,#26232,#26233,#26234,#26235,#26236,#26237,
#26238,#26239,#26240,#26241,#26242,#26243,#26244,#26245,#26246,#26247,#26248,
#26249,#26250,#26251,#26252,#26253,#26254,#26255),.UNSPECIFIED.,.F.,.F.)
B_SPLINE_CURVE_WITH_KNOTS((6,1,1,1,1,1,1,1,1,1,1,1,1,1,1,1,1,1,1,1,1,1,
1,1,1,1,1,1,1,1,1,1,1,1,1,1,1,1,1,1,1,1,1,1,1,1,1,1,1,1,1,1,1,1,1,1,1,1,
1,1,1,1,1,1,1,6),(-1.,-0.984615384615383,-0.969230769230768,-0.953846153846152,
-0.938461538461537,-0.923076923076922,-0.907692307692306,-0.892307692307691,
-0.876923076923076,-0.86153846153846,-0.846153846153845,-0.83076923076923,
-0.815384615384614,-0.799999999999999,-0.784615384615384,-0.769230769230768,
-0.753846153846153,-0.738461538461538,-0.723076923076922,-0.707692307692307,
-0.692307692307692,-0.676923076923076,-0.661538461538461,-0.646153846153846,
-0.63076923076923,-0.615384615384615,-0.6,-0.584615384615384,-0.569230769230769,
-0.553846153846154,-0.538461538461538,-0.523076923076923,-0.507692307692308,
-0.492307692307692,-0.476923076923077,-0.461538461538462,-0.446153846153846,
-0.430769230769231,-0.415384615384615,-0.4,-0.384615384615385,-0.369230769230769,
-0.353846153846154,-0.338461538461538,-0.323076923076923,-0.307692307692308,
-0.292307692307692,-0.276923076923077,-0.261538461538462,-0.246153846153846,
-0.230769230769231,-0.215384615384615,-0.2,-0.184615384615385,-0.169230769230769,
-0.153846153846154,-0.138461538461538,-0.123076923076923,-0.107692307692308,
-0.0923076923076923,-0.0769230769230769,-0.0615384615384615,-0.0461538461538462,
-0.0307692307692308,-0.0153846153846154,0.),.UNSPECIFIED.)
CURVE()
GEOMETRIC_REPRESENTATION_ITEM()
RATIONAL_B_SPLINE_CURVE((1.,1.,1.,1.,1.,1.,1.,1.,1.,1.,1.,1.,1.,1.,1.,1.,
1.,1.,1.,1.,1.,1.,1.,1.,1.,1.,1.,1.,1.,1.,1.,1.,1.,1.,1.,1.,1.,1.,1.,1.,
1.,1.,1.,1.,1.,1.,1.,1.,1.,1.,1.,1.,1.,1.,1.,1.,1.,1.,1.,1.,1.,1.,1.,1.,
1.,1.,1.,1.,1.,1.))
REPRESENTATION_ITEM('')
);
#100=(
BOUNDED_CURVE()
B_SPLINE_CURVE(5,(#26402,#26403,#26404,#26405,#26406,#26407,#26408,#26409,
#26410,#26411,#26412,#26413,#26414,#26415,#26416,#26417,#26418,#26419,#26420,
#26421,#26422,#26423,#26424,#26425,#26426,#26427,#26428,#26429,#26430,#26431,
#26432,#26433,#26434,#26435,#26436,#26437,#26438,#26439,#26440,#26441,#26442,
#26443,#26444,#26445,#26446,#26447,#26448,#26449,#26450,#26451,#26452,#26453,
#26454,#26455,#26456,#26457,#26458,#26459,#26460,#26461,#26462,#26463,#26464,
#26465,#26466,#26467,#26468,#26469,#26470,#26471),.UNSPECIFIED.,.F.,.F.)
B_SPLINE_CURVE_WITH_KNOTS((6,1,1,1,1,1,1,1,1,1,1,1,1,1,1,1,1,1,1,1,1,1,
1,1,1,1,1,1,1,1,1,1,1,1,1,1,1,1,1,1,1,1,1,1,1,1,1,1,1,1,1,1,1,1,1,1,1,1,
1,1,1,1,1,1,1,6),(-1.,-0.984615384615383,-0.969230769230768,-0.953846153846152,
-0.938461538461537,-0.923076923076922,-0.907692307692306,-0.892307692307691,
-0.876923076923076,-0.86153846153846,-0.846153846153845,-0.83076923076923,
-0.815384615384614,-0.799999999999999,-0.784615384615384,-0.769230769230768,
-0.753846153846153,-0.738461538461538,-0.723076923076922,-0.707692307692307,
-0.692307692307692,-0.676923076923076,-0.661538461538461,-0.646153846153846,
-0.63076923076923,-0.615384615384615,-0.6,-0.584615384615384,-0.569230769230769,
-0.553846153846154,-0.538461538461538,-0.523076923076923,-0.507692307692308,
-0.492307692307692,-0.476923076923077,-0.461538461538462,-0.446153846153846,
-0.430769230769231,-0.415384615384615,-0.4,-0.384615384615385,-0.369230769230769,
-0.353846153846154,-0.338461538461538,-0.323076923076923,-0.307692307692308,
-0.292307692307692,-0.276923076923077,-0.261538461538462,-0.246153846153846,
-0.230769230769231,-0.215384615384615,-0.2,-0.184615384615385,-0.169230769230769,
-0.153846153846154,-0.138461538461538,-0.123076923076923,-0.107692307692308,
-0.0923076923076923,-0.0769230769230769,-0.0615384615384615,-0.0461538461538462,
-0.0307692307692308,-0.0153846153846154,0.),.UNSPECIFIED.)
CURVE()
GEOMETRIC_REPRESENTATION_ITEM()
RATIONAL_B_SPLINE_CURVE((1.,1.,1.,1.,1.,1.,1.,1.,1.,1.,1.,1.,1.,1.,1.,1.,
1.,1.,1.,1.,1.,1.,1.,1.,1.,1.,1.,1.,1.,1.,1.,1.,1.,1.,1.,1.,1.,1.,1.,1.,
1.,1.,1.,1.,1.,1.,1.,1.,1.,1.,1.,1.,1.,1.,1.,1.,1.,1.,1.,1.,1.,1.,1.,1.,
1.,1.,1.,1.,1.,1.))
REPRESENTATION_ITEM('')
);
#101=(
BOUNDED_CURVE()
B_SPLINE_CURVE(5,(#26618,#26619,#26620,#26621,#26622,#26623,#26624,#26625,
#26626,#26627,#26628,#26629,#26630,#26631,#26632,#26633,#26634,#26635,#26636,
#26637,#26638,#26639,#26640,#26641,#26642,#26643,#26644,#26645,#26646,#26647,
#26648,#26649,#26650,#26651,#26652,#26653,#26654,#26655,#26656,#26657,#26658,
#26659,#26660,#26661,#26662,#26663,#26664,#26665,#26666,#26667,#26668,#26669,
#26670,#26671,#26672,#26673,#26674,#26675,#26676,#26677,#26678,#26679,#26680,
#26681,#26682,#26683,#26684,#26685,#26686,#26687),.UNSPECIFIED.,.F.,.F.)
B_SPLINE_CURVE_WITH_KNOTS((6,1,1,1,1,1,1,1,1,1,1,1,1,1,1,1,1,1,1,1,1,1,
1,1,1,1,1,1,1,1,1,1,1,1,1,1,1,1,1,1,1,1,1,1,1,1,1,1,1,1,1,1,1,1,1,1,1,1,
1,1,1,1,1,1,1,6),(-1.,-0.984615384615383,-0.969230769230768,-0.953846153846152,
-0.938461538461537,-0.923076923076922,-0.907692307692306,-0.892307692307691,
-0.876923076923076,-0.86153846153846,-0.846153846153845,-0.83076923076923,
-0.815384615384614,-0.799999999999999,-0.784615384615384,-0.769230769230768,
-0.753846153846153,-0.738461538461538,-0.723076923076922,-0.707692307692307,
-0.692307692307692,-0.676923076923076,-0.661538461538461,-0.646153846153846,
-0.63076923076923,-0.615384615384615,-0.6,-0.584615384615384,-0.569230769230769,
-0.553846153846154,-0.538461538461538,-0.523076923076923,-0.507692307692308,
-0.492307692307692,-0.476923076923077,-0.461538461538462,-0.446153846153846,
-0.430769230769231,-0.415384615384615,-0.4,-0.384615384615385,-0.369230769230769,
-0.353846153846154,-0.338461538461538,-0.323076923076923,-0.307692307692308,
-0.292307692307692,-0.276923076923077,-0.261538461538462,-0.246153846153846,
-0.230769230769231,-0.215384615384615,-0.2,-0.184615384615385,-0.169230769230769,
-0.153846153846154,-0.138461538461538,-0.123076923076923,-0.107692307692308,
-0.0923076923076923,-0.0769230769230769,-0.0615384615384615,-0.0461538461538462,
-0.0307692307692308,-0.0153846153846154,0.),.UNSPECIFIED.)
CURVE()
GEOMETRIC_REPRESENTATION_ITEM()
RATIONAL_B_SPLINE_CURVE((1.,1.,1.,1.,1.,1.,1.,1.,1.,1.,1.,1.,1.,1.,1.,1.,
1.,1.,1.,1.,1.,1.,1.,1.,1.,1.,1.,1.,1.,1.,1.,1.,1.,1.,1.,1.,1.,1.,1.,1.,
1.,1.,1.,1.,1.,1.,1.,1.,1.,1.,1.,1.,1.,1.,1.,1.,1.,1.,1.,1.,1.,1.,1.,1.,
1.,1.,1.,1.,1.,1.))
REPRESENTATION_ITEM('')
);
#102=(
BOUNDED_CURVE()
B_SPLINE_CURVE(5,(#26834,#26835,#26836,#26837,#26838,#26839,#26840,#26841,
#26842,#26843,#26844,#26845,#26846,#26847,#26848,#26849,#26850,#26851,#26852,
#26853,#26854,#26855,#26856,#26857,#26858,#26859,#26860,#26861,#26862,#26863,
#26864,#26865,#26866,#26867,#26868,#26869,#26870,#26871,#26872,#26873,#26874,
#26875,#26876,#26877,#26878,#26879,#26880,#26881,#26882,#26883,#26884,#26885,
#26886,#26887,#26888,#26889,#26890,#26891,#26892,#26893,#26894,#26895,#26896,
#26897,#26898,#26899,#26900,#26901,#26902,#26903),.UNSPECIFIED.,.F.,.F.)
B_SPLINE_CURVE_WITH_KNOTS((6,1,1,1,1,1,1,1,1,1,1,1,1,1,1,1,1,1,1,1,1,1,
1,1,1,1,1,1,1,1,1,1,1,1,1,1,1,1,1,1,1,1,1,1,1,1,1,1,1,1,1,1,1,1,1,1,1,1,
1,1,1,1,1,1,1,6),(-1.,-0.984615384615383,-0.969230769230768,-0.953846153846152,
-0.938461538461537,-0.923076923076922,-0.907692307692306,-0.892307692307691,
-0.876923076923076,-0.86153846153846,-0.846153846153845,-0.83076923076923,
-0.815384615384614,-0.799999999999999,-0.784615384615384,-0.769230769230768,
-0.753846153846153,-0.738461538461538,-0.723076923076922,-0.707692307692307,
-0.692307692307692,-0.676923076923076,-0.661538461538461,-0.646153846153846,
-0.63076923076923,-0.615384615384615,-0.6,-0.584615384615384,-0.569230769230769,
-0.553846153846154,-0.538461538461538,-0.523076923076923,-0.507692307692308,
-0.492307692307692,-0.476923076923077,-0.461538461538462,-0.446153846153846,
-0.430769230769231,-0.415384615384615,-0.4,-0.384615384615385,-0.369230769230769,
-0.353846153846154,-0.338461538461538,-0.323076923076923,-0.307692307692308,
-0.292307692307692,-0.276923076923077,-0.261538461538462,-0.246153846153846,
-0.230769230769231,-0.215384615384615,-0.2,-0.184615384615385,-0.169230769230769,
-0.153846153846154,-0.138461538461538,-0.123076923076923,-0.107692307692308,
-0.0923076923076923,-0.0769230769230769,-0.0615384615384615,-0.0461538461538462,
-0.0307692307692308,-0.0153846153846154,0.),.UNSPECIFIED.)
CURVE()
GEOMETRIC_REPRESENTATION_ITEM()
RATIONAL_B_SPLINE_CURVE((1.,1.,1.,1.,1.,1.,1.,1.,1.,1.,1.,1.,1.,1.,1.,1.,
1.,1.,1.,1.,1.,1.,1.,1.,1.,1.,1.,1.,1.,1.,1.,1.,1.,1.,1.,1.,1.,1.,1.,1.,
1.,1.,1.,1.,1.,1.,1.,1.,1.,1.,1.,1.,1.,1.,1.,1.,1.,1.,1.,1.,1.,1.,1.,1.,
1.,1.,1.,1.,1.,1.))
REPRESENTATION_ITEM('')
);
#103=(
BOUNDED_CURVE()
B_SPLINE_CURVE(5,(#27050,#27051,#27052,#27053,#27054,#27055,#27056,#27057,
#27058,#27059,#27060,#27061,#27062,#27063,#27064,#27065,#27066,#27067,#27068,
#27069,#27070,#27071,#27072,#27073,#27074,#27075,#27076,#27077,#27078,#27079,
#27080,#27081,#27082,#27083,#27084,#27085,#27086,#27087,#27088,#27089,#27090,
#27091,#27092,#27093,#27094,#27095,#27096,#27097,#27098,#27099,#27100,#27101,
#27102,#27103,#27104,#27105,#27106,#27107,#27108,#27109,#27110,#27111,#27112,
#27113,#27114,#27115,#27116,#27117,#27118,#27119),.UNSPECIFIED.,.F.,.F.)
B_SPLINE_CURVE_WITH_KNOTS((6,1,1,1,1,1,1,1,1,1,1,1,1,1,1,1,1,1,1,1,1,1,
1,1,1,1,1,1,1,1,1,1,1,1,1,1,1,1,1,1,1,1,1,1,1,1,1,1,1,1,1,1,1,1,1,1,1,1,
1,1,1,1,1,1,1,6),(-1.,-0.984615384615383,-0.969230769230768,-0.953846153846152,
-0.938461538461537,-0.923076923076922,-0.907692307692306,-0.892307692307691,
-0.876923076923076,-0.86153846153846,-0.846153846153845,-0.83076923076923,
-0.815384615384614,-0.799999999999999,-0.784615384615384,-0.769230769230768,
-0.753846153846153,-0.738461538461538,-0.723076923076922,-0.707692307692307,
-0.692307692307692,-0.676923076923076,-0.661538461538461,-0.646153846153846,
-0.63076923076923,-0.615384615384615,-0.6,-0.584615384615384,-0.569230769230769,
-0.553846153846154,-0.538461538461538,-0.523076923076923,-0.507692307692308,
-0.492307692307692,-0.476923076923077,-0.461538461538462,-0.446153846153846,
-0.430769230769231,-0.415384615384615,-0.4,-0.384615384615385,-0.369230769230769,
-0.353846153846154,-0.338461538461538,-0.323076923076923,-0.307692307692308,
-0.292307692307692,-0.276923076923077,-0.261538461538462,-0.246153846153846,
-0.230769230769231,-0.215384615384615,-0.2,-0.184615384615385,-0.169230769230769,
-0.153846153846154,-0.138461538461538,-0.123076923076923,-0.107692307692308,
-0.0923076923076923,-0.0769230769230769,-0.0615384615384615,-0.0461538461538462,
-0.0307692307692308,-0.0153846153846154,0.),.UNSPECIFIED.)
CURVE()
GEOMETRIC_REPRESENTATION_ITEM()
RATIONAL_B_SPLINE_CURVE((1.,1.,1.,1.,1.,1.,1.,1.,1.,1.,1.,1.,1.,1.,1.,1.,
1.,1.,1.,1.,1.,1.,1.,1.,1.,1.,1.,1.,1.,1.,1.,1.,1.,1.,1.,1.,1.,1.,1.,1.,
1.,1.,1.,1.,1.,1.,1.,1.,1.,1.,1.,1.,1.,1.,1.,1.,1.,1.,1.,1.,1.,1.,1.,1.,
1.,1.,1.,1.,1.,1.))
REPRESENTATION_ITEM('')
);
#104=(
BOUNDED_CURVE()
B_SPLINE_CURVE(5,(#27266,#27267,#27268,#27269,#27270,#27271,#27272,#27273,
#27274,#27275,#27276,#27277,#27278,#27279,#27280,#27281,#27282,#27283,#27284,
#27285,#27286,#27287,#27288,#27289,#27290,#27291,#27292,#27293,#27294,#27295,
#27296,#27297,#27298,#27299,#27300,#27301,#27302,#27303,#27304,#27305,#27306,
#27307,#27308,#27309,#27310,#27311,#27312,#27313,#27314,#27315,#27316,#27317,
#27318,#27319,#27320,#27321,#27322,#27323,#27324,#27325,#27326,#27327,#27328,
#27329,#27330,#27331,#27332,#27333,#27334,#27335),.UNSPECIFIED.,.F.,.F.)
B_SPLINE_CURVE_WITH_KNOTS((6,1,1,1,1,1,1,1,1,1,1,1,1,1,1,1,1,1,1,1,1,1,
1,1,1,1,1,1,1,1,1,1,1,1,1,1,1,1,1,1,1,1,1,1,1,1,1,1,1,1,1,1,1,1,1,1,1,1,
1,1,1,1,1,1,1,6),(-1.,-0.984615384615383,-0.969230769230768,-0.953846153846152,
-0.938461538461537,-0.923076923076922,-0.907692307692306,-0.892307692307691,
-0.876923076923076,-0.86153846153846,-0.846153846153845,-0.83076923076923,
-0.815384615384614,-0.799999999999999,-0.784615384615384,-0.769230769230768,
-0.753846153846153,-0.738461538461538,-0.723076923076922,-0.707692307692307,
-0.692307692307692,-0.676923076923076,-0.661538461538461,-0.646153846153846,
-0.63076923076923,-0.615384615384615,-0.6,-0.584615384615384,-0.569230769230769,
-0.553846153846154,-0.538461538461538,-0.523076923076923,-0.507692307692308,
-0.492307692307692,-0.476923076923077,-0.461538461538462,-0.446153846153846,
-0.430769230769231,-0.415384615384615,-0.4,-0.384615384615385,-0.369230769230769,
-0.353846153846154,-0.338461538461538,-0.323076923076923,-0.307692307692308,
-0.292307692307692,-0.276923076923077,-0.261538461538462,-0.246153846153846,
-0.230769230769231,-0.215384615384615,-0.2,-0.184615384615385,-0.169230769230769,
-0.153846153846154,-0.138461538461538,-0.123076923076923,-0.107692307692308,
-0.0923076923076923,-0.0769230769230769,-0.0615384615384615,-0.0461538461538462,
-0.0307692307692308,-0.0153846153846154,0.),.UNSPECIFIED.)
CURVE()
GEOMETRIC_REPRESENTATION_ITEM()
RATIONAL_B_SPLINE_CURVE((1.,1.,1.,1.,1.,1.,1.,1.,1.,1.,1.,1.,1.,1.,1.,1.,
1.,1.,1.,1.,1.,1.,1.,1.,1.,1.,1.,1.,1.,1.,1.,1.,1.,1.,1.,1.,1.,1.,1.,1.,
1.,1.,1.,1.,1.,1.,1.,1.,1.,1.,1.,1.,1.,1.,1.,1.,1.,1.,1.,1.,1.,1.,1.,1.,
1.,1.,1.,1.,1.,1.))
REPRESENTATION_ITEM('')
);
#105=(
BOUNDED_CURVE()
B_SPLINE_CURVE(5,(#27482,#27483,#27484,#27485,#27486,#27487,#27488,#27489,
#27490,#27491,#27492,#27493,#27494,#27495,#27496,#27497,#27498,#27499,#27500,
#27501,#27502,#27503,#27504,#27505,#27506,#27507,#27508,#27509,#27510,#27511,
#27512,#27513,#27514,#27515,#27516,#27517,#27518,#27519,#27520,#27521,#27522,
#27523,#27524,#27525,#27526,#27527,#27528,#27529,#27530,#27531,#27532,#27533,
#27534,#27535,#27536,#27537,#27538,#27539,#27540,#27541,#27542,#27543,#27544,
#27545,#27546,#27547,#27548,#27549,#27550,#27551),.UNSPECIFIED.,.F.,.F.)
B_SPLINE_CURVE_WITH_KNOTS((6,1,1,1,1,1,1,1,1,1,1,1,1,1,1,1,1,1,1,1,1,1,
1,1,1,1,1,1,1,1,1,1,1,1,1,1,1,1,1,1,1,1,1,1,1,1,1,1,1,1,1,1,1,1,1,1,1,1,
1,1,1,1,1,1,1,6),(-1.,-0.984615384615383,-0.969230769230768,-0.953846153846152,
-0.938461538461537,-0.923076923076922,-0.907692307692306,-0.892307692307691,
-0.876923076923076,-0.86153846153846,-0.846153846153845,-0.83076923076923,
-0.815384615384614,-0.799999999999999,-0.784615384615384,-0.769230769230768,
-0.753846153846153,-0.738461538461538,-0.723076923076922,-0.707692307692307,
-0.692307692307692,-0.676923076923076,-0.661538461538461,-0.646153846153846,
-0.63076923076923,-0.615384615384615,-0.6,-0.584615384615384,-0.569230769230769,
-0.553846153846154,-0.538461538461538,-0.523076923076923,-0.507692307692308,
-0.492307692307692,-0.476923076923077,-0.461538461538462,-0.446153846153846,
-0.430769230769231,-0.415384615384615,-0.4,-0.384615384615385,-0.369230769230769,
-0.353846153846154,-0.338461538461538,-0.323076923076923,-0.307692307692308,
-0.292307692307692,-0.276923076923077,-0.261538461538462,-0.246153846153846,
-0.230769230769231,-0.215384615384615,-0.2,-0.184615384615385,-0.169230769230769,
-0.153846153846154,-0.138461538461538,-0.123076923076923,-0.107692307692308,
-0.0923076923076923,-0.0769230769230769,-0.0615384615384615,-0.0461538461538462,
-0.0307692307692308,-0.0153846153846154,0.),.UNSPECIFIED.)
CURVE()
GEOMETRIC_REPRESENTATION_ITEM()
RATIONAL_B_SPLINE_CURVE((1.,1.,1.,1.,1.,1.,1.,1.,1.,1.,1.,1.,1.,1.,1.,1.,
1.,1.,1.,1.,1.,1.,1.,1.,1.,1.,1.,1.,1.,1.,1.,1.,1.,1.,1.,1.,1.,1.,1.,1.,
1.,1.,1.,1.,1.,1.,1.,1.,1.,1.,1.,1.,1.,1.,1.,1.,1.,1.,1.,1.,1.,1.,1.,1.,
1.,1.,1.,1.,1.,1.))
REPRESENTATION_ITEM('')
);
#106=(
BOUNDED_CURVE()
B_SPLINE_CURVE(5,(#27698,#27699,#27700,#27701,#27702,#27703,#27704,#27705,
#27706,#27707,#27708,#27709,#27710,#27711,#27712,#27713,#27714,#27715,#27716,
#27717,#27718,#27719,#27720,#27721,#27722,#27723,#27724,#27725,#27726,#27727,
#27728,#27729,#27730,#27731,#27732,#27733,#27734,#27735,#27736,#27737,#27738,
#27739,#27740,#27741,#27742,#27743,#27744,#27745,#27746,#27747,#27748,#27749,
#27750,#27751,#27752,#27753,#27754,#27755,#27756,#27757,#27758,#27759,#27760,
#27761,#27762,#27763,#27764,#27765,#27766,#27767),.UNSPECIFIED.,.F.,.F.)
B_SPLINE_CURVE_WITH_KNOTS((6,1,1,1,1,1,1,1,1,1,1,1,1,1,1,1,1,1,1,1,1,1,
1,1,1,1,1,1,1,1,1,1,1,1,1,1,1,1,1,1,1,1,1,1,1,1,1,1,1,1,1,1,1,1,1,1,1,1,
1,1,1,1,1,1,1,6),(-1.,-0.984615384615383,-0.969230769230768,-0.953846153846152,
-0.938461538461537,-0.923076923076922,-0.907692307692306,-0.892307692307691,
-0.876923076923076,-0.86153846153846,-0.846153846153845,-0.83076923076923,
-0.815384615384614,-0.799999999999999,-0.784615384615384,-0.769230769230768,
-0.753846153846153,-0.738461538461538,-0.723076923076922,-0.707692307692307,
-0.692307692307692,-0.676923076923076,-0.661538461538461,-0.646153846153846,
-0.63076923076923,-0.615384615384615,-0.6,-0.584615384615384,-0.569230769230769,
-0.553846153846154,-0.538461538461538,-0.523076923076923,-0.507692307692308,
-0.492307692307692,-0.476923076923077,-0.461538461538462,-0.446153846153846,
-0.430769230769231,-0.415384615384615,-0.4,-0.384615384615385,-0.369230769230769,
-0.353846153846154,-0.338461538461538,-0.323076923076923,-0.307692307692308,
-0.292307692307692,-0.276923076923077,-0.261538461538462,-0.246153846153846,
-0.230769230769231,-0.215384615384615,-0.2,-0.184615384615385,-0.169230769230769,
-0.153846153846154,-0.138461538461538,-0.123076923076923,-0.107692307692308,
-0.0923076923076923,-0.0769230769230769,-0.0615384615384615,-0.0461538461538462,
-0.0307692307692308,-0.0153846153846154,0.),.UNSPECIFIED.)
CURVE()
GEOMETRIC_REPRESENTATION_ITEM()
RATIONAL_B_SPLINE_CURVE((1.,1.,1.,1.,1.,1.,1.,1.,1.,1.,1.,1.,1.,1.,1.,1.,
1.,1.,1.,1.,1.,1.,1.,1.,1.,1.,1.,1.,1.,1.,1.,1.,1.,1.,1.,1.,1.,1.,1.,1.,
1.,1.,1.,1.,1.,1.,1.,1.,1.,1.,1.,1.,1.,1.,1.,1.,1.,1.,1.,1.,1.,1.,1.,1.,
1.,1.,1.,1.,1.,1.))
REPRESENTATION_ITEM('')
);
#107=(
BOUNDED_CURVE()
B_SPLINE_CURVE(5,(#27914,#27915,#27916,#27917,#27918,#27919,#27920,#27921,
#27922,#27923,#27924,#27925,#27926,#27927,#27928,#27929,#27930,#27931,#27932,
#27933,#27934,#27935,#27936,#27937,#27938,#27939,#27940,#27941,#27942,#27943,
#27944,#27945,#27946,#27947,#27948,#27949,#27950,#27951,#27952,#27953,#27954,
#27955,#27956,#27957,#27958,#27959,#27960,#27961,#27962,#27963,#27964,#27965,
#27966,#27967,#27968,#27969,#27970,#27971,#27972,#27973,#27974,#27975,#27976,
#27977,#27978,#27979,#27980,#27981,#27982,#27983),.UNSPECIFIED.,.F.,.F.)
B_SPLINE_CURVE_WITH_KNOTS((6,1,1,1,1,1,1,1,1,1,1,1,1,1,1,1,1,1,1,1,1,1,
1,1,1,1,1,1,1,1,1,1,1,1,1,1,1,1,1,1,1,1,1,1,1,1,1,1,1,1,1,1,1,1,1,1,1,1,
1,1,1,1,1,1,1,6),(-1.,-0.984615384615383,-0.969230769230768,-0.953846153846152,
-0.938461538461537,-0.923076923076922,-0.907692307692306,-0.892307692307691,
-0.876923076923076,-0.86153846153846,-0.846153846153845,-0.83076923076923,
-0.815384615384614,-0.799999999999999,-0.784615384615384,-0.769230769230768,
-0.753846153846153,-0.738461538461538,-0.723076923076922,-0.707692307692307,
-0.692307692307692,-0.676923076923076,-0.661538461538461,-0.646153846153846,
-0.63076923076923,-0.615384615384615,-0.6,-0.584615384615384,-0.569230769230769,
-0.553846153846154,-0.538461538461538,-0.523076923076923,-0.507692307692308,
-0.492307692307692,-0.476923076923077,-0.461538461538462,-0.446153846153846,
-0.430769230769231,-0.415384615384615,-0.4,-0.384615384615385,-0.369230769230769,
-0.353846153846154,-0.338461538461538,-0.323076923076923,-0.307692307692308,
-0.292307692307692,-0.276923076923077,-0.261538461538462,-0.246153846153846,
-0.230769230769231,-0.215384615384615,-0.2,-0.184615384615385,-0.169230769230769,
-0.153846153846154,-0.138461538461538,-0.123076923076923,-0.107692307692308,
-0.0923076923076923,-0.0769230769230769,-0.0615384615384615,-0.0461538461538462,
-0.0307692307692308,-0.0153846153846154,0.),.UNSPECIFIED.)
CURVE()
GEOMETRIC_REPRESENTATION_ITEM()
RATIONAL_B_SPLINE_CURVE((1.,1.,1.,1.,1.,1.,1.,1.,1.,1.,1.,1.,1.,1.,1.,1.,
1.,1.,1.,1.,1.,1.,1.,1.,1.,1.,1.,1.,1.,1.,1.,1.,1.,1.,1.,1.,1.,1.,1.,1.,
1.,1.,1.,1.,1.,1.,1.,1.,1.,1.,1.,1.,1.,1.,1.,1.,1.,1.,1.,1.,1.,1.,1.,1.,
1.,1.,1.,1.,1.,1.))
REPRESENTATION_ITEM('')
);
#108=(
BOUNDED_CURVE()
B_SPLINE_CURVE(5,(#28130,#28131,#28132,#28133,#28134,#28135,#28136,#28137,
#28138,#28139,#28140,#28141,#28142,#28143,#28144,#28145,#28146,#28147,#28148,
#28149,#28150,#28151,#28152,#28153,#28154,#28155,#28156,#28157,#28158,#28159,
#28160,#28161,#28162,#28163,#28164,#28165,#28166,#28167,#28168,#28169,#28170,
#28171,#28172,#28173,#28174,#28175,#28176,#28177,#28178,#28179,#28180,#28181,
#28182,#28183,#28184,#28185,#28186,#28187,#28188,#28189,#28190,#28191,#28192,
#28193,#28194,#28195,#28196,#28197,#28198,#28199),.UNSPECIFIED.,.F.,.F.)
B_SPLINE_CURVE_WITH_KNOTS((6,1,1,1,1,1,1,1,1,1,1,1,1,1,1,1,1,1,1,1,1,1,
1,1,1,1,1,1,1,1,1,1,1,1,1,1,1,1,1,1,1,1,1,1,1,1,1,1,1,1,1,1,1,1,1,1,1,1,
1,1,1,1,1,1,1,6),(-1.,-0.984615384615383,-0.969230769230768,-0.953846153846152,
-0.938461538461537,-0.923076923076922,-0.907692307692306,-0.892307692307691,
-0.876923076923076,-0.86153846153846,-0.846153846153845,-0.83076923076923,
-0.815384615384614,-0.799999999999999,-0.784615384615384,-0.769230769230768,
-0.753846153846153,-0.738461538461538,-0.723076923076922,-0.707692307692307,
-0.692307692307692,-0.676923076923076,-0.661538461538461,-0.646153846153846,
-0.63076923076923,-0.615384615384615,-0.6,-0.584615384615384,-0.569230769230769,
-0.553846153846154,-0.538461538461538,-0.523076923076923,-0.507692307692308,
-0.492307692307692,-0.476923076923077,-0.461538461538462,-0.446153846153846,
-0.430769230769231,-0.415384615384615,-0.4,-0.384615384615385,-0.369230769230769,
-0.353846153846154,-0.338461538461538,-0.323076923076923,-0.307692307692308,
-0.292307692307692,-0.276923076923077,-0.261538461538462,-0.246153846153846,
-0.230769230769231,-0.215384615384615,-0.2,-0.184615384615385,-0.169230769230769,
-0.153846153846154,-0.138461538461538,-0.123076923076923,-0.107692307692308,
-0.0923076923076923,-0.0769230769230769,-0.0615384615384615,-0.0461538461538462,
-0.0307692307692308,-0.0153846153846154,0.),.UNSPECIFIED.)
CURVE()
GEOMETRIC_REPRESENTATION_ITEM()
RATIONAL_B_SPLINE_CURVE((1.,1.,1.,1.,1.,1.,1.,1.,1.,1.,1.,1.,1.,1.,1.,1.,
1.,1.,1.,1.,1.,1.,1.,1.,1.,1.,1.,1.,1.,1.,1.,1.,1.,1.,1.,1.,1.,1.,1.,1.,
1.,1.,1.,1.,1.,1.,1.,1.,1.,1.,1.,1.,1.,1.,1.,1.,1.,1.,1.,1.,1.,1.,1.,1.,
1.,1.,1.,1.,1.,1.))
REPRESENTATION_ITEM('')
);
#109=(
BOUNDED_CURVE()
B_SPLINE_CURVE(5,(#28346,#28347,#28348,#28349,#28350,#28351,#28352,#28353,
#28354,#28355,#28356,#28357,#28358,#28359,#28360,#28361,#28362,#28363,#28364,
#28365,#28366,#28367,#28368,#28369,#28370,#28371,#28372,#28373,#28374,#28375,
#28376,#28377,#28378,#28379,#28380,#28381,#28382,#28383,#28384,#28385,#28386,
#28387,#28388,#28389,#28390,#28391,#28392,#28393,#28394,#28395,#28396,#28397,
#28398,#28399,#28400,#28401,#28402,#28403,#28404,#28405,#28406,#28407,#28408,
#28409,#28410,#28411,#28412,#28413,#28414,#28415),.UNSPECIFIED.,.F.,.F.)
B_SPLINE_CURVE_WITH_KNOTS((6,1,1,1,1,1,1,1,1,1,1,1,1,1,1,1,1,1,1,1,1,1,
1,1,1,1,1,1,1,1,1,1,1,1,1,1,1,1,1,1,1,1,1,1,1,1,1,1,1,1,1,1,1,1,1,1,1,1,
1,1,1,1,1,1,1,6),(-1.,-0.984615384615383,-0.969230769230768,-0.953846153846152,
-0.938461538461537,-0.923076923076922,-0.907692307692306,-0.892307692307691,
-0.876923076923076,-0.86153846153846,-0.846153846153845,-0.83076923076923,
-0.815384615384614,-0.799999999999999,-0.784615384615384,-0.769230769230768,
-0.753846153846153,-0.738461538461538,-0.723076923076922,-0.707692307692307,
-0.692307692307692,-0.676923076923076,-0.661538461538461,-0.646153846153846,
-0.63076923076923,-0.615384615384615,-0.6,-0.584615384615384,-0.569230769230769,
-0.553846153846154,-0.538461538461538,-0.523076923076923,-0.507692307692308,
-0.492307692307692,-0.476923076923077,-0.461538461538462,-0.446153846153846,
-0.430769230769231,-0.415384615384615,-0.4,-0.384615384615385,-0.369230769230769,
-0.353846153846154,-0.338461538461538,-0.323076923076923,-0.307692307692308,
-0.292307692307692,-0.276923076923077,-0.261538461538462,-0.246153846153846,
-0.230769230769231,-0.215384615384615,-0.2,-0.184615384615385,-0.169230769230769,
-0.153846153846154,-0.138461538461538,-0.123076923076923,-0.107692307692308,
-0.0923076923076923,-0.0769230769230769,-0.0615384615384615,-0.0461538461538462,
-0.0307692307692308,-0.0153846153846154,0.),.UNSPECIFIED.)
CURVE()
GEOMETRIC_REPRESENTATION_ITEM()
RATIONAL_B_SPLINE_CURVE((1.,1.,1.,1.,1.,1.,1.,1.,1.,1.,1.,1.,1.,1.,1.,1.,
1.,1.,1.,1.,1.,1.,1.,1.,1.,1.,1.,1.,1.,1.,1.,1.,1.,1.,1.,1.,1.,1.,1.,1.,
1.,1.,1.,1.,1.,1.,1.,1.,1.,1.,1.,1.,1.,1.,1.,1.,1.,1.,1.,1.,1.,1.,1.,1.,
1.,1.,1.,1.,1.,1.))
REPRESENTATION_ITEM('')
);
#110=(
BOUNDED_CURVE()
B_SPLINE_CURVE(5,(#28562,#28563,#28564,#28565,#28566,#28567,#28568,#28569,
#28570,#28571,#28572,#28573,#28574,#28575,#28576,#28577,#28578,#28579,#28580,
#28581,#28582,#28583,#28584,#28585,#28586,#28587,#28588,#28589,#28590,#28591,
#28592,#28593,#28594,#28595,#28596,#28597,#28598,#28599,#28600,#28601,#28602,
#28603,#28604,#28605,#28606,#28607,#28608,#28609,#28610,#28611,#28612,#28613,
#28614,#28615,#28616,#28617,#28618,#28619,#28620,#28621,#28622,#28623,#28624,
#28625,#28626,#28627,#28628,#28629,#28630,#28631),.UNSPECIFIED.,.F.,.F.)
B_SPLINE_CURVE_WITH_KNOTS((6,1,1,1,1,1,1,1,1,1,1,1,1,1,1,1,1,1,1,1,1,1,
1,1,1,1,1,1,1,1,1,1,1,1,1,1,1,1,1,1,1,1,1,1,1,1,1,1,1,1,1,1,1,1,1,1,1,1,
1,1,1,1,1,1,1,6),(-1.,-0.984615384615383,-0.969230769230768,-0.953846153846152,
-0.938461538461537,-0.923076923076922,-0.907692307692306,-0.892307692307691,
-0.876923076923076,-0.86153846153846,-0.846153846153845,-0.83076923076923,
-0.815384615384614,-0.799999999999999,-0.784615384615384,-0.769230769230768,
-0.753846153846153,-0.738461538461538,-0.723076923076922,-0.707692307692307,
-0.692307692307692,-0.676923076923076,-0.661538461538461,-0.646153846153846,
-0.63076923076923,-0.615384615384615,-0.6,-0.584615384615384,-0.569230769230769,
-0.553846153846154,-0.538461538461538,-0.523076923076923,-0.507692307692308,
-0.492307692307692,-0.476923076923077,-0.461538461538462,-0.446153846153846,
-0.430769230769231,-0.415384615384615,-0.4,-0.384615384615385,-0.369230769230769,
-0.353846153846154,-0.338461538461538,-0.323076923076923,-0.307692307692308,
-0.292307692307692,-0.276923076923077,-0.261538461538462,-0.246153846153846,
-0.230769230769231,-0.215384615384615,-0.2,-0.184615384615385,-0.169230769230769,
-0.153846153846154,-0.138461538461538,-0.123076923076923,-0.107692307692308,
-0.0923076923076923,-0.0769230769230769,-0.0615384615384615,-0.0461538461538462,
-0.0307692307692308,-0.0153846153846154,0.),.UNSPECIFIED.)
CURVE()
GEOMETRIC_REPRESENTATION_ITEM()
RATIONAL_B_SPLINE_CURVE((1.,1.,1.,1.,1.,1.,1.,1.,1.,1.,1.,1.,1.,1.,1.,1.,
1.,1.,1.,1.,1.,1.,1.,1.,1.,1.,1.,1.,1.,1.,1.,1.,1.,1.,1.,1.,1.,1.,1.,1.,
1.,1.,1.,1.,1.,1.,1.,1.,1.,1.,1.,1.,1.,1.,1.,1.,1.,1.,1.,1.,1.,1.,1.,1.,
1.,1.,1.,1.,1.,1.))
REPRESENTATION_ITEM('')
);
#111=(
BOUNDED_CURVE()
B_SPLINE_CURVE(5,(#28778,#28779,#28780,#28781,#28782,#28783,#28784,#28785,
#28786,#28787,#28788,#28789,#28790,#28791,#28792,#28793,#28794,#28795,#28796,
#28797,#28798,#28799,#28800,#28801,#28802,#28803,#28804,#28805,#28806,#28807,
#28808,#28809,#28810,#28811,#28812,#28813,#28814,#28815,#28816,#28817,#28818,
#28819,#28820,#28821,#28822,#28823,#28824,#28825,#28826,#28827,#28828,#28829,
#28830,#28831,#28832,#28833,#28834,#28835,#28836,#28837,#28838,#28839,#28840,
#28841,#28842,#28843,#28844,#28845,#28846,#28847),.UNSPECIFIED.,.F.,.F.)
B_SPLINE_CURVE_WITH_KNOTS((6,1,1,1,1,1,1,1,1,1,1,1,1,1,1,1,1,1,1,1,1,1,
1,1,1,1,1,1,1,1,1,1,1,1,1,1,1,1,1,1,1,1,1,1,1,1,1,1,1,1,1,1,1,1,1,1,1,1,
1,1,1,1,1,1,1,6),(-1.,-0.984615384615383,-0.969230769230768,-0.953846153846152,
-0.938461538461537,-0.923076923076922,-0.907692307692306,-0.892307692307691,
-0.876923076923076,-0.86153846153846,-0.846153846153845,-0.83076923076923,
-0.815384615384614,-0.799999999999999,-0.784615384615384,-0.769230769230768,
-0.753846153846153,-0.738461538461538,-0.723076923076922,-0.707692307692307,
-0.692307692307692,-0.676923076923076,-0.661538461538461,-0.646153846153846,
-0.63076923076923,-0.615384615384615,-0.6,-0.584615384615384,-0.569230769230769,
-0.553846153846154,-0.538461538461538,-0.523076923076923,-0.507692307692308,
-0.492307692307692,-0.476923076923077,-0.461538461538462,-0.446153846153846,
-0.430769230769231,-0.415384615384615,-0.4,-0.384615384615385,-0.369230769230769,
-0.353846153846154,-0.338461538461538,-0.323076923076923,-0.307692307692308,
-0.292307692307692,-0.276923076923077,-0.261538461538462,-0.246153846153846,
-0.230769230769231,-0.215384615384615,-0.2,-0.184615384615385,-0.169230769230769,
-0.153846153846154,-0.138461538461538,-0.123076923076923,-0.107692307692308,
-0.0923076923076923,-0.0769230769230769,-0.0615384615384615,-0.0461538461538462,
-0.0307692307692308,-0.0153846153846154,0.),.UNSPECIFIED.)
CURVE()
GEOMETRIC_REPRESENTATION_ITEM()
RATIONAL_B_SPLINE_CURVE((1.,1.,1.,1.,1.,1.,1.,1.,1.,1.,1.,1.,1.,1.,1.,1.,
1.,1.,1.,1.,1.,1.,1.,1.,1.,1.,1.,1.,1.,1.,1.,1.,1.,1.,1.,1.,1.,1.,1.,1.,
1.,1.,1.,1.,1.,1.,1.,1.,1.,1.,1.,1.,1.,1.,1.,1.,1.,1.,1.,1.,1.,1.,1.,1.,
1.,1.,1.,1.,1.,1.))
REPRESENTATION_ITEM('')
);
#112=(
BOUNDED_CURVE()
B_SPLINE_CURVE(5,(#28994,#28995,#28996,#28997,#28998,#28999,#29000,#29001,
#29002,#29003,#29004,#29005,#29006,#29007,#29008,#29009,#29010,#29011,#29012,
#29013,#29014,#29015,#29016,#29017,#29018,#29019,#29020,#29021,#29022,#29023,
#29024,#29025,#29026,#29027,#29028,#29029,#29030,#29031,#29032,#29033,#29034,
#29035,#29036,#29037,#29038,#29039,#29040,#29041,#29042,#29043,#29044,#29045,
#29046,#29047,#29048,#29049,#29050,#29051,#29052,#29053,#29054,#29055,#29056,
#29057,#29058,#29059,#29060,#29061,#29062,#29063),.UNSPECIFIED.,.F.,.F.)
B_SPLINE_CURVE_WITH_KNOTS((6,1,1,1,1,1,1,1,1,1,1,1,1,1,1,1,1,1,1,1,1,1,
1,1,1,1,1,1,1,1,1,1,1,1,1,1,1,1,1,1,1,1,1,1,1,1,1,1,1,1,1,1,1,1,1,1,1,1,
1,1,1,1,1,1,1,6),(-1.,-0.984615384615383,-0.969230769230768,-0.953846153846152,
-0.938461538461537,-0.923076923076922,-0.907692307692306,-0.892307692307691,
-0.876923076923076,-0.86153846153846,-0.846153846153845,-0.83076923076923,
-0.815384615384614,-0.799999999999999,-0.784615384615384,-0.769230769230768,
-0.753846153846153,-0.738461538461538,-0.723076923076922,-0.707692307692307,
-0.692307692307692,-0.676923076923076,-0.661538461538461,-0.646153846153846,
-0.63076923076923,-0.615384615384615,-0.6,-0.584615384615384,-0.569230769230769,
-0.553846153846154,-0.538461538461538,-0.523076923076923,-0.507692307692308,
-0.492307692307692,-0.476923076923077,-0.461538461538462,-0.446153846153846,
-0.430769230769231,-0.415384615384615,-0.4,-0.384615384615385,-0.369230769230769,
-0.353846153846154,-0.338461538461538,-0.323076923076923,-0.307692307692308,
-0.292307692307692,-0.276923076923077,-0.261538461538462,-0.246153846153846,
-0.230769230769231,-0.215384615384615,-0.2,-0.184615384615385,-0.169230769230769,
-0.153846153846154,-0.138461538461538,-0.123076923076923,-0.107692307692308,
-0.0923076923076923,-0.0769230769230769,-0.0615384615384615,-0.0461538461538462,
-0.0307692307692308,-0.0153846153846154,0.),.UNSPECIFIED.)
CURVE()
GEOMETRIC_REPRESENTATION_ITEM()
RATIONAL_B_SPLINE_CURVE((1.,1.,1.,1.,1.,1.,1.,1.,1.,1.,1.,1.,1.,1.,1.,1.,
1.,1.,1.,1.,1.,1.,1.,1.,1.,1.,1.,1.,1.,1.,1.,1.,1.,1.,1.,1.,1.,1.,1.,1.,
1.,1.,1.,1.,1.,1.,1.,1.,1.,1.,1.,1.,1.,1.,1.,1.,1.,1.,1.,1.,1.,1.,1.,1.,
1.,1.,1.,1.,1.,1.))
REPRESENTATION_ITEM('')
);
#113=(
BOUNDED_CURVE()
B_SPLINE_CURVE(5,(#29210,#29211,#29212,#29213,#29214,#29215,#29216,#29217,
#29218,#29219,#29220,#29221,#29222,#29223,#29224,#29225,#29226,#29227,#29228,
#29229,#29230,#29231,#29232,#29233,#29234,#29235,#29236,#29237,#29238,#29239,
#29240,#29241,#29242,#29243,#29244,#29245,#29246,#29247,#29248,#29249,#29250,
#29251,#29252,#29253,#29254,#29255,#29256,#29257,#29258,#29259,#29260,#29261,
#29262,#29263,#29264,#29265,#29266,#29267,#29268,#29269,#29270,#29271,#29272,
#29273,#29274,#29275,#29276,#29277,#29278,#29279),.UNSPECIFIED.,.F.,.F.)
B_SPLINE_CURVE_WITH_KNOTS((6,1,1,1,1,1,1,1,1,1,1,1,1,1,1,1,1,1,1,1,1,1,
1,1,1,1,1,1,1,1,1,1,1,1,1,1,1,1,1,1,1,1,1,1,1,1,1,1,1,1,1,1,1,1,1,1,1,1,
1,1,1,1,1,1,1,6),(-1.,-0.984615384615383,-0.969230769230768,-0.953846153846152,
-0.938461538461537,-0.923076923076922,-0.907692307692306,-0.892307692307691,
-0.876923076923076,-0.86153846153846,-0.846153846153845,-0.83076923076923,
-0.815384615384614,-0.799999999999999,-0.784615384615384,-0.769230769230768,
-0.753846153846153,-0.738461538461538,-0.723076923076922,-0.707692307692307,
-0.692307692307692,-0.676923076923076,-0.661538461538461,-0.646153846153846,
-0.63076923076923,-0.615384615384615,-0.6,-0.584615384615384,-0.569230769230769,
-0.553846153846154,-0.538461538461538,-0.523076923076923,-0.507692307692308,
-0.492307692307692,-0.476923076923077,-0.461538461538462,-0.446153846153846,
-0.430769230769231,-0.415384615384615,-0.4,-0.384615384615385,-0.369230769230769,
-0.353846153846154,-0.338461538461538,-0.323076923076923,-0.307692307692308,
-0.292307692307692,-0.276923076923077,-0.261538461538462,-0.246153846153846,
-0.230769230769231,-0.215384615384615,-0.2,-0.184615384615385,-0.169230769230769,
-0.153846153846154,-0.138461538461538,-0.123076923076923,-0.107692307692308,
-0.0923076923076923,-0.0769230769230769,-0.0615384615384615,-0.0461538461538462,
-0.0307692307692308,-0.0153846153846154,0.),.UNSPECIFIED.)
CURVE()
GEOMETRIC_REPRESENTATION_ITEM()
RATIONAL_B_SPLINE_CURVE((1.,1.,1.,1.,1.,1.,1.,1.,1.,1.,1.,1.,1.,1.,1.,1.,
1.,1.,1.,1.,1.,1.,1.,1.,1.,1.,1.,1.,1.,1.,1.,1.,1.,1.,1.,1.,1.,1.,1.,1.,
1.,1.,1.,1.,1.,1.,1.,1.,1.,1.,1.,1.,1.,1.,1.,1.,1.,1.,1.,1.,1.,1.,1.,1.,
1.,1.,1.,1.,1.,1.))
REPRESENTATION_ITEM('')
);
#114=(
BOUNDED_CURVE()
B_SPLINE_CURVE(5,(#29426,#29427,#29428,#29429,#29430,#29431,#29432,#29433,
#29434,#29435,#29436,#29437,#29438,#29439,#29440,#29441,#29442,#29443,#29444,
#29445,#29446,#29447,#29448,#29449,#29450,#29451,#29452,#29453,#29454,#29455,
#29456,#29457,#29458,#29459,#29460,#29461,#29462,#29463,#29464,#29465,#29466,
#29467,#29468,#29469,#29470,#29471,#29472,#29473,#29474,#29475,#29476,#29477,
#29478,#29479,#29480,#29481,#29482,#29483,#29484,#29485,#29486,#29487,#29488,
#29489,#29490,#29491,#29492,#29493,#29494,#29495),.UNSPECIFIED.,.F.,.F.)
B_SPLINE_CURVE_WITH_KNOTS((6,1,1,1,1,1,1,1,1,1,1,1,1,1,1,1,1,1,1,1,1,1,
1,1,1,1,1,1,1,1,1,1,1,1,1,1,1,1,1,1,1,1,1,1,1,1,1,1,1,1,1,1,1,1,1,1,1,1,
1,1,1,1,1,1,1,6),(-1.,-0.984615384615383,-0.969230769230768,-0.953846153846152,
-0.938461538461537,-0.923076923076922,-0.907692307692306,-0.892307692307691,
-0.876923076923076,-0.86153846153846,-0.846153846153845,-0.83076923076923,
-0.815384615384614,-0.799999999999999,-0.784615384615384,-0.769230769230768,
-0.753846153846153,-0.738461538461538,-0.723076923076922,-0.707692307692307,
-0.692307692307692,-0.676923076923076,-0.661538461538461,-0.646153846153846,
-0.63076923076923,-0.615384615384615,-0.6,-0.584615384615384,-0.569230769230769,
-0.553846153846154,-0.538461538461538,-0.523076923076923,-0.507692307692308,
-0.492307692307692,-0.476923076923077,-0.461538461538462,-0.446153846153846,
-0.430769230769231,-0.415384615384615,-0.4,-0.384615384615385,-0.369230769230769,
-0.353846153846154,-0.338461538461538,-0.323076923076923,-0.307692307692308,
-0.292307692307692,-0.276923076923077,-0.261538461538462,-0.246153846153846,
-0.230769230769231,-0.215384615384615,-0.2,-0.184615384615385,-0.169230769230769,
-0.153846153846154,-0.138461538461538,-0.123076923076923,-0.107692307692308,
-0.0923076923076923,-0.0769230769230769,-0.0615384615384615,-0.0461538461538462,
-0.0307692307692308,-0.0153846153846154,0.),.UNSPECIFIED.)
CURVE()
GEOMETRIC_REPRESENTATION_ITEM()
RATIONAL_B_SPLINE_CURVE((1.,1.,1.,1.,1.,1.,1.,1.,1.,1.,1.,1.,1.,1.,1.,1.,
1.,1.,1.,1.,1.,1.,1.,1.,1.,1.,1.,1.,1.,1.,1.,1.,1.,1.,1.,1.,1.,1.,1.,1.,
1.,1.,1.,1.,1.,1.,1.,1.,1.,1.,1.,1.,1.,1.,1.,1.,1.,1.,1.,1.,1.,1.,1.,1.,
1.,1.,1.,1.,1.,1.))
REPRESENTATION_ITEM('')
);
#115=(
BOUNDED_CURVE()
B_SPLINE_CURVE(5,(#29642,#29643,#29644,#29645,#29646,#29647,#29648,#29649,
#29650,#29651,#29652,#29653,#29654,#29655,#29656,#29657,#29658,#29659,#29660,
#29661,#29662,#29663,#29664,#29665,#29666,#29667,#29668,#29669,#29670,#29671,
#29672,#29673,#29674,#29675,#29676,#29677,#29678,#29679,#29680,#29681,#29682,
#29683,#29684,#29685,#29686,#29687,#29688,#29689,#29690,#29691,#29692,#29693,
#29694,#29695,#29696,#29697,#29698,#29699,#29700,#29701,#29702,#29703,#29704,
#29705,#29706,#29707,#29708,#29709,#29710,#29711),.UNSPECIFIED.,.F.,.F.)
B_SPLINE_CURVE_WITH_KNOTS((6,1,1,1,1,1,1,1,1,1,1,1,1,1,1,1,1,1,1,1,1,1,
1,1,1,1,1,1,1,1,1,1,1,1,1,1,1,1,1,1,1,1,1,1,1,1,1,1,1,1,1,1,1,1,1,1,1,1,
1,1,1,1,1,1,1,6),(-1.,-0.984615384615383,-0.969230769230768,-0.953846153846152,
-0.938461538461537,-0.923076923076922,-0.907692307692306,-0.892307692307691,
-0.876923076923076,-0.86153846153846,-0.846153846153845,-0.83076923076923,
-0.815384615384614,-0.799999999999999,-0.784615384615384,-0.769230769230768,
-0.753846153846153,-0.738461538461538,-0.723076923076922,-0.707692307692307,
-0.692307692307692,-0.676923076923076,-0.661538461538461,-0.646153846153846,
-0.63076923076923,-0.615384615384615,-0.6,-0.584615384615384,-0.569230769230769,
-0.553846153846154,-0.538461538461538,-0.523076923076923,-0.507692307692308,
-0.492307692307692,-0.476923076923077,-0.461538461538462,-0.446153846153846,
-0.430769230769231,-0.415384615384615,-0.4,-0.384615384615385,-0.369230769230769,
-0.353846153846154,-0.338461538461538,-0.323076923076923,-0.307692307692308,
-0.292307692307692,-0.276923076923077,-0.261538461538462,-0.246153846153846,
-0.230769230769231,-0.215384615384615,-0.2,-0.184615384615385,-0.169230769230769,
-0.153846153846154,-0.138461538461538,-0.123076923076923,-0.107692307692308,
-0.0923076923076923,-0.0769230769230769,-0.0615384615384615,-0.0461538461538462,
-0.0307692307692308,-0.0153846153846154,0.),.UNSPECIFIED.)
CURVE()
GEOMETRIC_REPRESENTATION_ITEM()
RATIONAL_B_SPLINE_CURVE((1.,1.,1.,1.,1.,1.,1.,1.,1.,1.,1.,1.,1.,1.,1.,1.,
1.,1.,1.,1.,1.,1.,1.,1.,1.,1.,1.,1.,1.,1.,1.,1.,1.,1.,1.,1.,1.,1.,1.,1.,
1.,1.,1.,1.,1.,1.,1.,1.,1.,1.,1.,1.,1.,1.,1.,1.,1.,1.,1.,1.,1.,1.,1.,1.,
1.,1.,1.,1.,1.,1.))
REPRESENTATION_ITEM('')
);
#116=(
BOUNDED_CURVE()
B_SPLINE_CURVE(5,(#29858,#29859,#29860,#29861,#29862,#29863,#29864,#29865,
#29866,#29867,#29868,#29869,#29870,#29871,#29872,#29873,#29874,#29875,#29876,
#29877,#29878,#29879,#29880,#29881,#29882,#29883,#29884,#29885,#29886,#29887,
#29888,#29889,#29890,#29891,#29892,#29893,#29894,#29895,#29896,#29897,#29898,
#29899,#29900,#29901,#29902,#29903,#29904,#29905,#29906,#29907,#29908,#29909,
#29910,#29911,#29912,#29913,#29914,#29915,#29916,#29917,#29918,#29919,#29920,
#29921,#29922,#29923,#29924,#29925,#29926,#29927),.UNSPECIFIED.,.F.,.F.)
B_SPLINE_CURVE_WITH_KNOTS((6,1,1,1,1,1,1,1,1,1,1,1,1,1,1,1,1,1,1,1,1,1,
1,1,1,1,1,1,1,1,1,1,1,1,1,1,1,1,1,1,1,1,1,1,1,1,1,1,1,1,1,1,1,1,1,1,1,1,
1,1,1,1,1,1,1,6),(-1.,-0.984615384615383,-0.969230769230768,-0.953846153846152,
-0.938461538461537,-0.923076923076922,-0.907692307692306,-0.892307692307691,
-0.876923076923076,-0.86153846153846,-0.846153846153845,-0.83076923076923,
-0.815384615384614,-0.799999999999999,-0.784615384615384,-0.769230769230768,
-0.753846153846153,-0.738461538461538,-0.723076923076922,-0.707692307692307,
-0.692307692307692,-0.676923076923076,-0.661538461538461,-0.646153846153846,
-0.63076923076923,-0.615384615384615,-0.6,-0.584615384615384,-0.569230769230769,
-0.553846153846154,-0.538461538461538,-0.523076923076923,-0.507692307692308,
-0.492307692307692,-0.476923076923077,-0.461538461538462,-0.446153846153846,
-0.430769230769231,-0.415384615384615,-0.4,-0.384615384615385,-0.369230769230769,
-0.353846153846154,-0.338461538461538,-0.323076923076923,-0.307692307692308,
-0.292307692307692,-0.276923076923077,-0.261538461538462,-0.246153846153846,
-0.230769230769231,-0.215384615384615,-0.2,-0.184615384615385,-0.169230769230769,
-0.153846153846154,-0.138461538461538,-0.123076923076923,-0.107692307692308,
-0.0923076923076923,-0.0769230769230769,-0.0615384615384615,-0.0461538461538462,
-0.0307692307692308,-0.0153846153846154,0.),.UNSPECIFIED.)
CURVE()
GEOMETRIC_REPRESENTATION_ITEM()
RATIONAL_B_SPLINE_CURVE((1.,1.,1.,1.,1.,1.,1.,1.,1.,1.,1.,1.,1.,1.,1.,1.,
1.,1.,1.,1.,1.,1.,1.,1.,1.,1.,1.,1.,1.,1.,1.,1.,1.,1.,1.,1.,1.,1.,1.,1.,
1.,1.,1.,1.,1.,1.,1.,1.,1.,1.,1.,1.,1.,1.,1.,1.,1.,1.,1.,1.,1.,1.,1.,1.,
1.,1.,1.,1.,1.,1.))
REPRESENTATION_ITEM('')
);
#117=(
BOUNDED_CURVE()
B_SPLINE_CURVE(5,(#30074,#30075,#30076,#30077,#30078,#30079,#30080,#30081,
#30082,#30083,#30084,#30085,#30086,#30087,#30088,#30089,#30090,#30091,#30092,
#30093,#30094,#30095,#30096,#30097,#30098,#30099,#30100,#30101,#30102,#30103,
#30104,#30105,#30106,#30107,#30108,#30109,#30110,#30111,#30112,#30113,#30114,
#30115,#30116,#30117,#30118,#30119,#30120,#30121,#30122,#30123,#30124,#30125,
#30126,#30127,#30128,#30129,#30130,#30131,#30132,#30133,#30134,#30135,#30136,
#30137,#30138,#30139,#30140,#30141,#30142,#30143),.UNSPECIFIED.,.F.,.F.)
B_SPLINE_CURVE_WITH_KNOTS((6,1,1,1,1,1,1,1,1,1,1,1,1,1,1,1,1,1,1,1,1,1,
1,1,1,1,1,1,1,1,1,1,1,1,1,1,1,1,1,1,1,1,1,1,1,1,1,1,1,1,1,1,1,1,1,1,1,1,
1,1,1,1,1,1,1,6),(-1.,-0.984615384615383,-0.969230769230768,-0.953846153846152,
-0.938461538461537,-0.923076923076922,-0.907692307692306,-0.892307692307691,
-0.876923076923076,-0.86153846153846,-0.846153846153845,-0.83076923076923,
-0.815384615384614,-0.799999999999999,-0.784615384615384,-0.769230769230768,
-0.753846153846153,-0.738461538461538,-0.723076923076922,-0.707692307692307,
-0.692307692307692,-0.676923076923076,-0.661538461538461,-0.646153846153846,
-0.63076923076923,-0.615384615384615,-0.6,-0.584615384615384,-0.569230769230769,
-0.553846153846154,-0.538461538461538,-0.523076923076923,-0.507692307692308,
-0.492307692307692,-0.476923076923077,-0.461538461538462,-0.446153846153846,
-0.430769230769231,-0.415384615384615,-0.4,-0.384615384615385,-0.369230769230769,
-0.353846153846154,-0.338461538461538,-0.323076923076923,-0.307692307692308,
-0.292307692307692,-0.276923076923077,-0.261538461538462,-0.246153846153846,
-0.230769230769231,-0.215384615384615,-0.2,-0.184615384615385,-0.169230769230769,
-0.153846153846154,-0.138461538461538,-0.123076923076923,-0.107692307692308,
-0.0923076923076923,-0.0769230769230769,-0.0615384615384615,-0.0461538461538462,
-0.0307692307692308,-0.0153846153846154,0.),.UNSPECIFIED.)
CURVE()
GEOMETRIC_REPRESENTATION_ITEM()
RATIONAL_B_SPLINE_CURVE((1.,1.,1.,1.,1.,1.,1.,1.,1.,1.,1.,1.,1.,1.,1.,1.,
1.,1.,1.,1.,1.,1.,1.,1.,1.,1.,1.,1.,1.,1.,1.,1.,1.,1.,1.,1.,1.,1.,1.,1.,
1.,1.,1.,1.,1.,1.,1.,1.,1.,1.,1.,1.,1.,1.,1.,1.,1.,1.,1.,1.,1.,1.,1.,1.,
1.,1.,1.,1.,1.,1.))
REPRESENTATION_ITEM('')
);
#118=(
BOUNDED_CURVE()
B_SPLINE_CURVE(5,(#30290,#30291,#30292,#30293,#30294,#30295,#30296,#30297,
#30298,#30299,#30300,#30301,#30302,#30303,#30304,#30305,#30306,#30307,#30308,
#30309,#30310,#30311,#30312,#30313,#30314,#30315,#30316,#30317,#30318,#30319,
#30320,#30321,#30322,#30323,#30324,#30325,#30326,#30327,#30328,#30329,#30330,
#30331,#30332,#30333,#30334,#30335,#30336,#30337,#30338,#30339,#30340,#30341,
#30342,#30343,#30344,#30345,#30346,#30347,#30348,#30349,#30350,#30351,#30352,
#30353,#30354,#30355,#30356,#30357,#30358,#30359),.UNSPECIFIED.,.F.,.F.)
B_SPLINE_CURVE_WITH_KNOTS((6,1,1,1,1,1,1,1,1,1,1,1,1,1,1,1,1,1,1,1,1,1,
1,1,1,1,1,1,1,1,1,1,1,1,1,1,1,1,1,1,1,1,1,1,1,1,1,1,1,1,1,1,1,1,1,1,1,1,
1,1,1,1,1,1,1,6),(-1.,-0.984615384615383,-0.969230769230768,-0.953846153846152,
-0.938461538461537,-0.923076923076922,-0.907692307692306,-0.892307692307691,
-0.876923076923076,-0.86153846153846,-0.846153846153845,-0.83076923076923,
-0.815384615384614,-0.799999999999999,-0.784615384615384,-0.769230769230768,
-0.753846153846153,-0.738461538461538,-0.723076923076922,-0.707692307692307,
-0.692307692307692,-0.676923076923076,-0.661538461538461,-0.646153846153846,
-0.63076923076923,-0.615384615384615,-0.6,-0.584615384615384,-0.569230769230769,
-0.553846153846154,-0.538461538461538,-0.523076923076923,-0.507692307692308,
-0.492307692307692,-0.476923076923077,-0.461538461538462,-0.446153846153846,
-0.430769230769231,-0.415384615384615,-0.4,-0.384615384615385,-0.369230769230769,
-0.353846153846154,-0.338461538461538,-0.323076923076923,-0.307692307692308,
-0.292307692307692,-0.276923076923077,-0.261538461538462,-0.246153846153846,
-0.230769230769231,-0.215384615384615,-0.2,-0.184615384615385,-0.169230769230769,
-0.153846153846154,-0.138461538461538,-0.123076923076923,-0.107692307692308,
-0.0923076923076923,-0.0769230769230769,-0.0615384615384615,-0.0461538461538462,
-0.0307692307692308,-0.0153846153846154,0.),.UNSPECIFIED.)
CURVE()
GEOMETRIC_REPRESENTATION_ITEM()
RATIONAL_B_SPLINE_CURVE((1.,1.,1.,1.,1.,1.,1.,1.,1.,1.,1.,1.,1.,1.,1.,1.,
1.,1.,1.,1.,1.,1.,1.,1.,1.,1.,1.,1.,1.,1.,1.,1.,1.,1.,1.,1.,1.,1.,1.,1.,
1.,1.,1.,1.,1.,1.,1.,1.,1.,1.,1.,1.,1.,1.,1.,1.,1.,1.,1.,1.,1.,1.,1.,1.,
1.,1.,1.,1.,1.,1.))
REPRESENTATION_ITEM('')
);
#119=(
BOUNDED_CURVE()
B_SPLINE_CURVE(5,(#30506,#30507,#30508,#30509,#30510,#30511,#30512,#30513,
#30514,#30515,#30516,#30517,#30518,#30519,#30520,#30521,#30522,#30523,#30524,
#30525,#30526,#30527,#30528,#30529,#30530,#30531,#30532,#30533,#30534,#30535,
#30536,#30537,#30538,#30539,#30540,#30541,#30542,#30543,#30544,#30545,#30546,
#30547,#30548,#30549,#30550,#30551,#30552,#30553,#30554,#30555,#30556,#30557,
#30558,#30559,#30560,#30561,#30562,#30563,#30564,#30565,#30566,#30567,#30568,
#30569,#30570,#30571,#30572,#30573,#30574,#30575),.UNSPECIFIED.,.F.,.F.)
B_SPLINE_CURVE_WITH_KNOTS((6,1,1,1,1,1,1,1,1,1,1,1,1,1,1,1,1,1,1,1,1,1,
1,1,1,1,1,1,1,1,1,1,1,1,1,1,1,1,1,1,1,1,1,1,1,1,1,1,1,1,1,1,1,1,1,1,1,1,
1,1,1,1,1,1,1,6),(-1.,-0.984615384615383,-0.969230769230768,-0.953846153846152,
-0.938461538461537,-0.923076923076922,-0.907692307692306,-0.892307692307691,
-0.876923076923076,-0.86153846153846,-0.846153846153845,-0.83076923076923,
-0.815384615384614,-0.799999999999999,-0.784615384615384,-0.769230769230768,
-0.753846153846153,-0.738461538461538,-0.723076923076922,-0.707692307692307,
-0.692307692307692,-0.676923076923076,-0.661538461538461,-0.646153846153846,
-0.63076923076923,-0.615384615384615,-0.6,-0.584615384615384,-0.569230769230769,
-0.553846153846154,-0.538461538461538,-0.523076923076923,-0.507692307692308,
-0.492307692307692,-0.476923076923077,-0.461538461538462,-0.446153846153846,
-0.430769230769231,-0.415384615384615,-0.4,-0.384615384615385,-0.369230769230769,
-0.353846153846154,-0.338461538461538,-0.323076923076923,-0.307692307692308,
-0.292307692307692,-0.276923076923077,-0.261538461538462,-0.246153846153846,
-0.230769230769231,-0.215384615384615,-0.2,-0.184615384615385,-0.169230769230769,
-0.153846153846154,-0.138461538461538,-0.123076923076923,-0.107692307692308,
-0.0923076923076923,-0.0769230769230769,-0.0615384615384615,-0.0461538461538462,
-0.0307692307692308,-0.0153846153846154,0.),.UNSPECIFIED.)
CURVE()
GEOMETRIC_REPRESENTATION_ITEM()
RATIONAL_B_SPLINE_CURVE((1.,1.,1.,1.,1.,1.,1.,1.,1.,1.,1.,1.,1.,1.,1.,1.,
1.,1.,1.,1.,1.,1.,1.,1.,1.,1.,1.,1.,1.,1.,1.,1.,1.,1.,1.,1.,1.,1.,1.,1.,
1.,1.,1.,1.,1.,1.,1.,1.,1.,1.,1.,1.,1.,1.,1.,1.,1.,1.,1.,1.,1.,1.,1.,1.,
1.,1.,1.,1.,1.,1.))
REPRESENTATION_ITEM('')
);
#120=(
BOUNDED_CURVE()
B_SPLINE_CURVE(5,(#30722,#30723,#30724,#30725,#30726,#30727,#30728,#30729,
#30730,#30731,#30732,#30733,#30734,#30735,#30736,#30737,#30738,#30739,#30740,
#30741,#30742,#30743,#30744,#30745,#30746,#30747,#30748,#30749,#30750,#30751,
#30752,#30753,#30754,#30755,#30756,#30757,#30758,#30759,#30760,#30761,#30762,
#30763,#30764,#30765,#30766,#30767,#30768,#30769,#30770,#30771,#30772,#30773,
#30774,#30775,#30776,#30777,#30778,#30779,#30780,#30781,#30782,#30783,#30784,
#30785,#30786,#30787,#30788,#30789,#30790,#30791),.UNSPECIFIED.,.F.,.F.)
B_SPLINE_CURVE_WITH_KNOTS((6,1,1,1,1,1,1,1,1,1,1,1,1,1,1,1,1,1,1,1,1,1,
1,1,1,1,1,1,1,1,1,1,1,1,1,1,1,1,1,1,1,1,1,1,1,1,1,1,1,1,1,1,1,1,1,1,1,1,
1,1,1,1,1,1,1,6),(-1.,-0.984615384615383,-0.969230769230768,-0.953846153846152,
-0.938461538461537,-0.923076923076922,-0.907692307692306,-0.892307692307691,
-0.876923076923076,-0.86153846153846,-0.846153846153845,-0.83076923076923,
-0.815384615384614,-0.799999999999999,-0.784615384615384,-0.769230769230768,
-0.753846153846153,-0.738461538461538,-0.723076923076922,-0.707692307692307,
-0.692307692307692,-0.676923076923076,-0.661538461538461,-0.646153846153846,
-0.63076923076923,-0.615384615384615,-0.6,-0.584615384615384,-0.569230769230769,
-0.553846153846154,-0.538461538461538,-0.523076923076923,-0.507692307692308,
-0.492307692307692,-0.476923076923077,-0.461538461538462,-0.446153846153846,
-0.430769230769231,-0.415384615384615,-0.4,-0.384615384615385,-0.369230769230769,
-0.353846153846154,-0.338461538461538,-0.323076923076923,-0.307692307692308,
-0.292307692307692,-0.276923076923077,-0.261538461538462,-0.246153846153846,
-0.230769230769231,-0.215384615384615,-0.2,-0.184615384615385,-0.169230769230769,
-0.153846153846154,-0.138461538461538,-0.123076923076923,-0.107692307692308,
-0.0923076923076923,-0.0769230769230769,-0.0615384615384615,-0.0461538461538462,
-0.0307692307692308,-0.0153846153846154,0.),.UNSPECIFIED.)
CURVE()
GEOMETRIC_REPRESENTATION_ITEM()
RATIONAL_B_SPLINE_CURVE((1.,1.,1.,1.,1.,1.,1.,1.,1.,1.,1.,1.,1.,1.,1.,1.,
1.,1.,1.,1.,1.,1.,1.,1.,1.,1.,1.,1.,1.,1.,1.,1.,1.,1.,1.,1.,1.,1.,1.,1.,
1.,1.,1.,1.,1.,1.,1.,1.,1.,1.,1.,1.,1.,1.,1.,1.,1.,1.,1.,1.,1.,1.,1.,1.,
1.,1.,1.,1.,1.,1.))
REPRESENTATION_ITEM('')
);
#121=(
BOUNDED_CURVE()
B_SPLINE_CURVE(5,(#30938,#30939,#30940,#30941,#30942,#30943,#30944,#30945,
#30946,#30947,#30948,#30949,#30950,#30951,#30952,#30953,#30954,#30955,#30956,
#30957,#30958,#30959,#30960,#30961,#30962,#30963,#30964,#30965,#30966,#30967,
#30968,#30969,#30970,#30971,#30972,#30973,#30974,#30975,#30976,#30977,#30978,
#30979,#30980,#30981,#30982,#30983,#30984,#30985,#30986,#30987,#30988,#30989,
#30990,#30991,#30992,#30993,#30994,#30995,#30996,#30997,#30998,#30999,#31000,
#31001,#31002,#31003,#31004,#31005,#31006,#31007),.UNSPECIFIED.,.F.,.F.)
B_SPLINE_CURVE_WITH_KNOTS((6,1,1,1,1,1,1,1,1,1,1,1,1,1,1,1,1,1,1,1,1,1,
1,1,1,1,1,1,1,1,1,1,1,1,1,1,1,1,1,1,1,1,1,1,1,1,1,1,1,1,1,1,1,1,1,1,1,1,
1,1,1,1,1,1,1,6),(-1.,-0.984615384615383,-0.969230769230768,-0.953846153846152,
-0.938461538461537,-0.923076923076922,-0.907692307692306,-0.892307692307691,
-0.876923076923076,-0.86153846153846,-0.846153846153845,-0.83076923076923,
-0.815384615384614,-0.799999999999999,-0.784615384615384,-0.769230769230768,
-0.753846153846153,-0.738461538461538,-0.723076923076922,-0.707692307692307,
-0.692307692307692,-0.676923076923076,-0.661538461538461,-0.646153846153846,
-0.63076923076923,-0.615384615384615,-0.6,-0.584615384615384,-0.569230769230769,
-0.553846153846154,-0.538461538461538,-0.523076923076923,-0.507692307692308,
-0.492307692307692,-0.476923076923077,-0.461538461538462,-0.446153846153846,
-0.430769230769231,-0.415384615384615,-0.4,-0.384615384615385,-0.369230769230769,
-0.353846153846154,-0.338461538461538,-0.323076923076923,-0.307692307692308,
-0.292307692307692,-0.276923076923077,-0.261538461538462,-0.246153846153846,
-0.230769230769231,-0.215384615384615,-0.2,-0.184615384615385,-0.169230769230769,
-0.153846153846154,-0.138461538461538,-0.123076923076923,-0.107692307692308,
-0.0923076923076923,-0.0769230769230769,-0.0615384615384615,-0.0461538461538462,
-0.0307692307692308,-0.0153846153846154,0.),.UNSPECIFIED.)
CURVE()
GEOMETRIC_REPRESENTATION_ITEM()
RATIONAL_B_SPLINE_CURVE((1.,1.,1.,1.,1.,1.,1.,1.,1.,1.,1.,1.,1.,1.,1.,1.,
1.,1.,1.,1.,1.,1.,1.,1.,1.,1.,1.,1.,1.,1.,1.,1.,1.,1.,1.,1.,1.,1.,1.,1.,
1.,1.,1.,1.,1.,1.,1.,1.,1.,1.,1.,1.,1.,1.,1.,1.,1.,1.,1.,1.,1.,1.,1.,1.,
1.,1.,1.,1.,1.,1.))
REPRESENTATION_ITEM('')
);
#122=(
BOUNDED_CURVE()
B_SPLINE_CURVE(5,(#31154,#31155,#31156,#31157,#31158,#31159,#31160,#31161,
#31162,#31163,#31164,#31165,#31166,#31167,#31168,#31169,#31170,#31171,#31172,
#31173,#31174,#31175,#31176,#31177,#31178,#31179,#31180,#31181,#31182,#31183,
#31184,#31185,#31186,#31187,#31188,#31189,#31190,#31191,#31192,#31193,#31194,
#31195,#31196,#31197,#31198,#31199,#31200,#31201,#31202,#31203,#31204,#31205,
#31206,#31207,#31208,#31209,#31210,#31211,#31212,#31213,#31214,#31215,#31216,
#31217,#31218,#31219,#31220,#31221,#31222,#31223),.UNSPECIFIED.,.F.,.F.)
B_SPLINE_CURVE_WITH_KNOTS((6,1,1,1,1,1,1,1,1,1,1,1,1,1,1,1,1,1,1,1,1,1,
1,1,1,1,1,1,1,1,1,1,1,1,1,1,1,1,1,1,1,1,1,1,1,1,1,1,1,1,1,1,1,1,1,1,1,1,
1,1,1,1,1,1,1,6),(-1.,-0.984615384615383,-0.969230769230768,-0.953846153846152,
-0.938461538461537,-0.923076923076922,-0.907692307692306,-0.892307692307691,
-0.876923076923076,-0.86153846153846,-0.846153846153845,-0.83076923076923,
-0.815384615384614,-0.799999999999999,-0.784615384615384,-0.769230769230768,
-0.753846153846153,-0.738461538461538,-0.723076923076922,-0.707692307692307,
-0.692307692307692,-0.676923076923076,-0.661538461538461,-0.646153846153846,
-0.63076923076923,-0.615384615384615,-0.6,-0.584615384615384,-0.569230769230769,
-0.553846153846154,-0.538461538461538,-0.523076923076923,-0.507692307692308,
-0.492307692307692,-0.476923076923077,-0.461538461538462,-0.446153846153846,
-0.430769230769231,-0.415384615384615,-0.4,-0.384615384615385,-0.369230769230769,
-0.353846153846154,-0.338461538461538,-0.323076923076923,-0.307692307692308,
-0.292307692307692,-0.276923076923077,-0.261538461538462,-0.246153846153846,
-0.230769230769231,-0.215384615384615,-0.2,-0.184615384615385,-0.169230769230769,
-0.153846153846154,-0.138461538461538,-0.123076923076923,-0.107692307692308,
-0.0923076923076923,-0.0769230769230769,-0.0615384615384615,-0.0461538461538462,
-0.0307692307692308,-0.0153846153846154,0.),.UNSPECIFIED.)
CURVE()
GEOMETRIC_REPRESENTATION_ITEM()
RATIONAL_B_SPLINE_CURVE((1.,1.,1.,1.,1.,1.,1.,1.,1.,1.,1.,1.,1.,1.,1.,1.,
1.,1.,1.,1.,1.,1.,1.,1.,1.,1.,1.,1.,1.,1.,1.,1.,1.,1.,1.,1.,1.,1.,1.,1.,
1.,1.,1.,1.,1.,1.,1.,1.,1.,1.,1.,1.,1.,1.,1.,1.,1.,1.,1.,1.,1.,1.,1.,1.,
1.,1.,1.,1.,1.,1.))
REPRESENTATION_ITEM('')
);
#123=(
BOUNDED_CURVE()
B_SPLINE_CURVE(5,(#31370,#31371,#31372,#31373,#31374,#31375,#31376,#31377,
#31378,#31379,#31380,#31381,#31382,#31383,#31384,#31385,#31386,#31387,#31388,
#31389,#31390,#31391,#31392,#31393,#31394,#31395,#31396,#31397,#31398,#31399,
#31400,#31401,#31402,#31403,#31404,#31405,#31406,#31407,#31408,#31409,#31410,
#31411,#31412,#31413,#31414,#31415,#31416,#31417,#31418,#31419,#31420,#31421,
#31422,#31423,#31424,#31425,#31426,#31427,#31428,#31429,#31430,#31431,#31432,
#31433,#31434,#31435,#31436,#31437,#31438,#31439),.UNSPECIFIED.,.F.,.F.)
B_SPLINE_CURVE_WITH_KNOTS((6,1,1,1,1,1,1,1,1,1,1,1,1,1,1,1,1,1,1,1,1,1,
1,1,1,1,1,1,1,1,1,1,1,1,1,1,1,1,1,1,1,1,1,1,1,1,1,1,1,1,1,1,1,1,1,1,1,1,
1,1,1,1,1,1,1,6),(-1.,-0.984615384615383,-0.969230769230768,-0.953846153846152,
-0.938461538461537,-0.923076923076922,-0.907692307692306,-0.892307692307691,
-0.876923076923076,-0.86153846153846,-0.846153846153845,-0.83076923076923,
-0.815384615384614,-0.799999999999999,-0.784615384615384,-0.769230769230768,
-0.753846153846153,-0.738461538461538,-0.723076923076922,-0.707692307692307,
-0.692307692307692,-0.676923076923076,-0.661538461538461,-0.646153846153846,
-0.63076923076923,-0.615384615384615,-0.6,-0.584615384615384,-0.569230769230769,
-0.553846153846154,-0.538461538461538,-0.523076923076923,-0.507692307692308,
-0.492307692307692,-0.476923076923077,-0.461538461538462,-0.446153846153846,
-0.430769230769231,-0.415384615384615,-0.4,-0.384615384615385,-0.369230769230769,
-0.353846153846154,-0.338461538461538,-0.323076923076923,-0.307692307692308,
-0.292307692307692,-0.276923076923077,-0.261538461538462,-0.246153846153846,
-0.230769230769231,-0.215384615384615,-0.2,-0.184615384615385,-0.169230769230769,
-0.153846153846154,-0.138461538461538,-0.123076923076923,-0.107692307692308,
-0.0923076923076923,-0.0769230769230769,-0.0615384615384615,-0.0461538461538462,
-0.0307692307692308,-0.0153846153846154,0.),.UNSPECIFIED.)
CURVE()
GEOMETRIC_REPRESENTATION_ITEM()
RATIONAL_B_SPLINE_CURVE((1.,1.,1.,1.,1.,1.,1.,1.,1.,1.,1.,1.,1.,1.,1.,1.,
1.,1.,1.,1.,1.,1.,1.,1.,1.,1.,1.,1.,1.,1.,1.,1.,1.,1.,1.,1.,1.,1.,1.,1.,
1.,1.,1.,1.,1.,1.,1.,1.,1.,1.,1.,1.,1.,1.,1.,1.,1.,1.,1.,1.,1.,1.,1.,1.,
1.,1.,1.,1.,1.,1.))
REPRESENTATION_ITEM('')
);
#124=(
BOUNDED_CURVE()
B_SPLINE_CURVE(5,(#31586,#31587,#31588,#31589,#31590,#31591,#31592,#31593,
#31594,#31595,#31596,#31597,#31598,#31599,#31600,#31601,#31602,#31603,#31604,
#31605,#31606,#31607,#31608,#31609,#31610,#31611,#31612,#31613,#31614,#31615,
#31616,#31617,#31618,#31619,#31620,#31621,#31622,#31623,#31624,#31625,#31626,
#31627,#31628,#31629,#31630,#31631,#31632,#31633,#31634,#31635,#31636,#31637,
#31638,#31639,#31640,#31641,#31642,#31643,#31644,#31645,#31646,#31647,#31648,
#31649,#31650,#31651,#31652,#31653,#31654,#31655),.UNSPECIFIED.,.F.,.F.)
B_SPLINE_CURVE_WITH_KNOTS((6,1,1,1,1,1,1,1,1,1,1,1,1,1,1,1,1,1,1,1,1,1,
1,1,1,1,1,1,1,1,1,1,1,1,1,1,1,1,1,1,1,1,1,1,1,1,1,1,1,1,1,1,1,1,1,1,1,1,
1,1,1,1,1,1,1,6),(-1.,-0.984615384615383,-0.969230769230768,-0.953846153846152,
-0.938461538461537,-0.923076923076922,-0.907692307692306,-0.892307692307691,
-0.876923076923076,-0.86153846153846,-0.846153846153845,-0.83076923076923,
-0.815384615384614,-0.799999999999999,-0.784615384615384,-0.769230769230768,
-0.753846153846153,-0.738461538461538,-0.723076923076922,-0.707692307692307,
-0.692307692307692,-0.676923076923076,-0.661538461538461,-0.646153846153846,
-0.63076923076923,-0.615384615384615,-0.6,-0.584615384615384,-0.569230769230769,
-0.553846153846154,-0.538461538461538,-0.523076923076923,-0.507692307692308,
-0.492307692307692,-0.476923076923077,-0.461538461538462,-0.446153846153846,
-0.430769230769231,-0.415384615384615,-0.4,-0.384615384615385,-0.369230769230769,
-0.353846153846154,-0.338461538461538,-0.323076923076923,-0.307692307692308,
-0.292307692307692,-0.276923076923077,-0.261538461538462,-0.246153846153846,
-0.230769230769231,-0.215384615384615,-0.2,-0.184615384615385,-0.169230769230769,
-0.153846153846154,-0.138461538461538,-0.123076923076923,-0.107692307692308,
-0.0923076923076923,-0.0769230769230769,-0.0615384615384615,-0.0461538461538462,
-0.0307692307692308,-0.0153846153846154,0.),.UNSPECIFIED.)
CURVE()
GEOMETRIC_REPRESENTATION_ITEM()
RATIONAL_B_SPLINE_CURVE((1.,1.,1.,1.,1.,1.,1.,1.,1.,1.,1.,1.,1.,1.,1.,1.,
1.,1.,1.,1.,1.,1.,1.,1.,1.,1.,1.,1.,1.,1.,1.,1.,1.,1.,1.,1.,1.,1.,1.,1.,
1.,1.,1.,1.,1.,1.,1.,1.,1.,1.,1.,1.,1.,1.,1.,1.,1.,1.,1.,1.,1.,1.,1.,1.,
1.,1.,1.,1.,1.,1.))
REPRESENTATION_ITEM('')
);
#125=(
BOUNDED_CURVE()
B_SPLINE_CURVE(5,(#31802,#31803,#31804,#31805,#31806,#31807,#31808,#31809,
#31810,#31811,#31812,#31813,#31814,#31815,#31816,#31817,#31818,#31819,#31820,
#31821,#31822,#31823,#31824,#31825,#31826,#31827,#31828,#31829,#31830,#31831,
#31832,#31833,#31834,#31835,#31836,#31837,#31838,#31839,#31840,#31841,#31842,
#31843,#31844,#31845,#31846,#31847,#31848,#31849,#31850,#31851,#31852,#31853,
#31854,#31855,#31856,#31857,#31858,#31859,#31860,#31861,#31862,#31863,#31864,
#31865,#31866,#31867,#31868,#31869,#31870,#31871),.UNSPECIFIED.,.F.,.F.)
B_SPLINE_CURVE_WITH_KNOTS((6,1,1,1,1,1,1,1,1,1,1,1,1,1,1,1,1,1,1,1,1,1,
1,1,1,1,1,1,1,1,1,1,1,1,1,1,1,1,1,1,1,1,1,1,1,1,1,1,1,1,1,1,1,1,1,1,1,1,
1,1,1,1,1,1,1,6),(-1.,-0.984615384615383,-0.969230769230768,-0.953846153846152,
-0.938461538461537,-0.923076923076922,-0.907692307692306,-0.892307692307691,
-0.876923076923076,-0.86153846153846,-0.846153846153845,-0.83076923076923,
-0.815384615384614,-0.799999999999999,-0.784615384615384,-0.769230769230768,
-0.753846153846153,-0.738461538461538,-0.723076923076922,-0.707692307692307,
-0.692307692307692,-0.676923076923076,-0.661538461538461,-0.646153846153846,
-0.63076923076923,-0.615384615384615,-0.6,-0.584615384615384,-0.569230769230769,
-0.553846153846154,-0.538461538461538,-0.523076923076923,-0.507692307692308,
-0.492307692307692,-0.476923076923077,-0.461538461538462,-0.446153846153846,
-0.430769230769231,-0.415384615384615,-0.4,-0.384615384615385,-0.369230769230769,
-0.353846153846154,-0.338461538461538,-0.323076923076923,-0.307692307692308,
-0.292307692307692,-0.276923076923077,-0.261538461538462,-0.246153846153846,
-0.230769230769231,-0.215384615384615,-0.2,-0.184615384615385,-0.169230769230769,
-0.153846153846154,-0.138461538461538,-0.123076923076923,-0.107692307692308,
-0.0923076923076923,-0.0769230769230769,-0.0615384615384615,-0.0461538461538462,
-0.0307692307692308,-0.0153846153846154,0.),.UNSPECIFIED.)
CURVE()
GEOMETRIC_REPRESENTATION_ITEM()
RATIONAL_B_SPLINE_CURVE((1.,1.,1.,1.,1.,1.,1.,1.,1.,1.,1.,1.,1.,1.,1.,1.,
1.,1.,1.,1.,1.,1.,1.,1.,1.,1.,1.,1.,1.,1.,1.,1.,1.,1.,1.,1.,1.,1.,1.,1.,
1.,1.,1.,1.,1.,1.,1.,1.,1.,1.,1.,1.,1.,1.,1.,1.,1.,1.,1.,1.,1.,1.,1.,1.,
1.,1.,1.,1.,1.,1.))
REPRESENTATION_ITEM('')
);
#126=(
BOUNDED_CURVE()
B_SPLINE_CURVE(5,(#32018,#32019,#32020,#32021,#32022,#32023,#32024,#32025,
#32026,#32027,#32028,#32029,#32030,#32031,#32032,#32033,#32034,#32035,#32036,
#32037,#32038,#32039,#32040,#32041,#32042,#32043,#32044,#32045,#32046,#32047,
#32048,#32049,#32050,#32051,#32052,#32053,#32054,#32055,#32056,#32057,#32058,
#32059,#32060,#32061,#32062,#32063,#32064,#32065,#32066,#32067,#32068,#32069,
#32070,#32071,#32072,#32073,#32074,#32075,#32076,#32077,#32078,#32079,#32080,
#32081,#32082,#32083,#32084,#32085,#32086,#32087),.UNSPECIFIED.,.F.,.F.)
B_SPLINE_CURVE_WITH_KNOTS((6,1,1,1,1,1,1,1,1,1,1,1,1,1,1,1,1,1,1,1,1,1,
1,1,1,1,1,1,1,1,1,1,1,1,1,1,1,1,1,1,1,1,1,1,1,1,1,1,1,1,1,1,1,1,1,1,1,1,
1,1,1,1,1,1,1,6),(-1.,-0.984615384615383,-0.969230769230768,-0.953846153846152,
-0.938461538461537,-0.923076923076922,-0.907692307692306,-0.892307692307691,
-0.876923076923076,-0.86153846153846,-0.846153846153845,-0.83076923076923,
-0.815384615384614,-0.799999999999999,-0.784615384615384,-0.769230769230768,
-0.753846153846153,-0.738461538461538,-0.723076923076922,-0.707692307692307,
-0.692307692307692,-0.676923076923076,-0.661538461538461,-0.646153846153846,
-0.63076923076923,-0.615384615384615,-0.6,-0.584615384615384,-0.569230769230769,
-0.553846153846154,-0.538461538461538,-0.523076923076923,-0.507692307692308,
-0.492307692307692,-0.476923076923077,-0.461538461538462,-0.446153846153846,
-0.430769230769231,-0.415384615384615,-0.4,-0.384615384615385,-0.369230769230769,
-0.353846153846154,-0.338461538461538,-0.323076923076923,-0.307692307692308,
-0.292307692307692,-0.276923076923077,-0.261538461538462,-0.246153846153846,
-0.230769230769231,-0.215384615384615,-0.2,-0.184615384615385,-0.169230769230769,
-0.153846153846154,-0.138461538461538,-0.123076923076923,-0.107692307692308,
-0.0923076923076923,-0.0769230769230769,-0.0615384615384615,-0.0461538461538462,
-0.0307692307692308,-0.0153846153846154,0.),.UNSPECIFIED.)
CURVE()
GEOMETRIC_REPRESENTATION_ITEM()
RATIONAL_B_SPLINE_CURVE((1.,1.,1.,1.,1.,1.,1.,1.,1.,1.,1.,1.,1.,1.,1.,1.,
1.,1.,1.,1.,1.,1.,1.,1.,1.,1.,1.,1.,1.,1.,1.,1.,1.,1.,1.,1.,1.,1.,1.,1.,
1.,1.,1.,1.,1.,1.,1.,1.,1.,1.,1.,1.,1.,1.,1.,1.,1.,1.,1.,1.,1.,1.,1.,1.,
1.,1.,1.,1.,1.,1.))
REPRESENTATION_ITEM('')
);
#127=(
BOUNDED_CURVE()
B_SPLINE_CURVE(5,(#32234,#32235,#32236,#32237,#32238,#32239,#32240,#32241,
#32242,#32243,#32244,#32245,#32246,#32247,#32248,#32249,#32250,#32251,#32252,
#32253,#32254,#32255,#32256,#32257,#32258,#32259,#32260,#32261,#32262,#32263,
#32264,#32265,#32266,#32267,#32268,#32269,#32270,#32271,#32272,#32273,#32274,
#32275,#32276,#32277,#32278,#32279,#32280,#32281,#32282,#32283,#32284,#32285,
#32286,#32287,#32288,#32289,#32290,#32291,#32292,#32293,#32294,#32295,#32296,
#32297,#32298,#32299,#32300,#32301,#32302,#32303),.UNSPECIFIED.,.F.,.F.)
B_SPLINE_CURVE_WITH_KNOTS((6,1,1,1,1,1,1,1,1,1,1,1,1,1,1,1,1,1,1,1,1,1,
1,1,1,1,1,1,1,1,1,1,1,1,1,1,1,1,1,1,1,1,1,1,1,1,1,1,1,1,1,1,1,1,1,1,1,1,
1,1,1,1,1,1,1,6),(-1.,-0.984615384615383,-0.969230769230768,-0.953846153846152,
-0.938461538461537,-0.923076923076922,-0.907692307692306,-0.892307692307691,
-0.876923076923076,-0.86153846153846,-0.846153846153845,-0.83076923076923,
-0.815384615384614,-0.799999999999999,-0.784615384615384,-0.769230769230768,
-0.753846153846153,-0.738461538461538,-0.723076923076922,-0.707692307692307,
-0.692307692307692,-0.676923076923076,-0.661538461538461,-0.646153846153846,
-0.63076923076923,-0.615384615384615,-0.6,-0.584615384615384,-0.569230769230769,
-0.553846153846154,-0.538461538461538,-0.523076923076923,-0.507692307692308,
-0.492307692307692,-0.476923076923077,-0.461538461538462,-0.446153846153846,
-0.430769230769231,-0.415384615384615,-0.4,-0.384615384615385,-0.369230769230769,
-0.353846153846154,-0.338461538461538,-0.323076923076923,-0.307692307692308,
-0.292307692307692,-0.276923076923077,-0.261538461538462,-0.246153846153846,
-0.230769230769231,-0.215384615384615,-0.2,-0.184615384615385,-0.169230769230769,
-0.153846153846154,-0.138461538461538,-0.123076923076923,-0.107692307692308,
-0.0923076923076923,-0.0769230769230769,-0.0615384615384615,-0.0461538461538462,
-0.0307692307692308,-0.0153846153846154,0.),.UNSPECIFIED.)
CURVE()
GEOMETRIC_REPRESENTATION_ITEM()
RATIONAL_B_SPLINE_CURVE((1.,1.,1.,1.,1.,1.,1.,1.,1.,1.,1.,1.,1.,1.,1.,1.,
1.,1.,1.,1.,1.,1.,1.,1.,1.,1.,1.,1.,1.,1.,1.,1.,1.,1.,1.,1.,1.,1.,1.,1.,
1.,1.,1.,1.,1.,1.,1.,1.,1.,1.,1.,1.,1.,1.,1.,1.,1.,1.,1.,1.,1.,1.,1.,1.,
1.,1.,1.,1.,1.,1.))
REPRESENTATION_ITEM('')
);
#128=(
BOUNDED_CURVE()
B_SPLINE_CURVE(5,(#32450,#32451,#32452,#32453,#32454,#32455,#32456,#32457,
#32458,#32459,#32460,#32461,#32462,#32463,#32464,#32465,#32466,#32467,#32468,
#32469,#32470,#32471,#32472,#32473,#32474,#32475,#32476,#32477,#32478,#32479,
#32480,#32481,#32482,#32483,#32484,#32485,#32486,#32487,#32488,#32489,#32490,
#32491,#32492,#32493,#32494,#32495,#32496,#32497,#32498,#32499,#32500,#32501,
#32502,#32503,#32504,#32505,#32506,#32507,#32508,#32509,#32510,#32511,#32512,
#32513,#32514,#32515,#32516,#32517,#32518,#32519),.UNSPECIFIED.,.F.,.F.)
B_SPLINE_CURVE_WITH_KNOTS((6,1,1,1,1,1,1,1,1,1,1,1,1,1,1,1,1,1,1,1,1,1,
1,1,1,1,1,1,1,1,1,1,1,1,1,1,1,1,1,1,1,1,1,1,1,1,1,1,1,1,1,1,1,1,1,1,1,1,
1,1,1,1,1,1,1,6),(-1.,-0.984615384615383,-0.969230769230768,-0.953846153846152,
-0.938461538461537,-0.923076923076922,-0.907692307692306,-0.892307692307691,
-0.876923076923076,-0.86153846153846,-0.846153846153845,-0.83076923076923,
-0.815384615384614,-0.799999999999999,-0.784615384615384,-0.769230769230768,
-0.753846153846153,-0.738461538461538,-0.723076923076922,-0.707692307692307,
-0.692307692307692,-0.676923076923076,-0.661538461538461,-0.646153846153846,
-0.63076923076923,-0.615384615384615,-0.6,-0.584615384615384,-0.569230769230769,
-0.553846153846154,-0.538461538461538,-0.523076923076923,-0.507692307692308,
-0.492307692307692,-0.476923076923077,-0.461538461538462,-0.446153846153846,
-0.430769230769231,-0.415384615384615,-0.4,-0.384615384615385,-0.369230769230769,
-0.353846153846154,-0.338461538461538,-0.323076923076923,-0.307692307692308,
-0.292307692307692,-0.276923076923077,-0.261538461538462,-0.246153846153846,
-0.230769230769231,-0.215384615384615,-0.2,-0.184615384615385,-0.169230769230769,
-0.153846153846154,-0.138461538461538,-0.123076923076923,-0.107692307692308,
-0.0923076923076923,-0.0769230769230769,-0.0615384615384615,-0.0461538461538462,
-0.0307692307692308,-0.0153846153846154,0.),.UNSPECIFIED.)
CURVE()
GEOMETRIC_REPRESENTATION_ITEM()
RATIONAL_B_SPLINE_CURVE((1.,1.,1.,1.,1.,1.,1.,1.,1.,1.,1.,1.,1.,1.,1.,1.,
1.,1.,1.,1.,1.,1.,1.,1.,1.,1.,1.,1.,1.,1.,1.,1.,1.,1.,1.,1.,1.,1.,1.,1.,
1.,1.,1.,1.,1.,1.,1.,1.,1.,1.,1.,1.,1.,1.,1.,1.,1.,1.,1.,1.,1.,1.,1.,1.,
1.,1.,1.,1.,1.,1.))
REPRESENTATION_ITEM('')
);
#129=(
BOUNDED_CURVE()
B_SPLINE_CURVE(5,(#32666,#32667,#32668,#32669,#32670,#32671,#32672,#32673,
#32674,#32675,#32676,#32677,#32678,#32679,#32680,#32681,#32682,#32683,#32684,
#32685,#32686,#32687,#32688,#32689,#32690,#32691,#32692,#32693,#32694,#32695,
#32696,#32697,#32698,#32699,#32700,#32701,#32702,#32703,#32704,#32705,#32706,
#32707,#32708,#32709,#32710,#32711,#32712,#32713,#32714,#32715,#32716,#32717,
#32718,#32719,#32720,#32721,#32722,#32723,#32724,#32725,#32726,#32727,#32728,
#32729,#32730,#32731,#32732,#32733,#32734,#32735),.UNSPECIFIED.,.F.,.F.)
B_SPLINE_CURVE_WITH_KNOTS((6,1,1,1,1,1,1,1,1,1,1,1,1,1,1,1,1,1,1,1,1,1,
1,1,1,1,1,1,1,1,1,1,1,1,1,1,1,1,1,1,1,1,1,1,1,1,1,1,1,1,1,1,1,1,1,1,1,1,
1,1,1,1,1,1,1,6),(-1.,-0.984615384615383,-0.969230769230768,-0.953846153846152,
-0.938461538461537,-0.923076923076922,-0.907692307692306,-0.892307692307691,
-0.876923076923076,-0.86153846153846,-0.846153846153845,-0.83076923076923,
-0.815384615384614,-0.799999999999999,-0.784615384615384,-0.769230769230768,
-0.753846153846153,-0.738461538461538,-0.723076923076922,-0.707692307692307,
-0.692307692307692,-0.676923076923076,-0.661538461538461,-0.646153846153846,
-0.63076923076923,-0.615384615384615,-0.6,-0.584615384615384,-0.569230769230769,
-0.553846153846154,-0.538461538461538,-0.523076923076923,-0.507692307692308,
-0.492307692307692,-0.476923076923077,-0.461538461538462,-0.446153846153846,
-0.430769230769231,-0.415384615384615,-0.4,-0.384615384615385,-0.369230769230769,
-0.353846153846154,-0.338461538461538,-0.323076923076923,-0.307692307692308,
-0.292307692307692,-0.276923076923077,-0.261538461538462,-0.246153846153846,
-0.230769230769231,-0.215384615384615,-0.2,-0.184615384615385,-0.169230769230769,
-0.153846153846154,-0.138461538461538,-0.123076923076923,-0.107692307692308,
-0.0923076923076923,-0.0769230769230769,-0.0615384615384615,-0.0461538461538462,
-0.0307692307692308,-0.0153846153846154,0.),.UNSPECIFIED.)
CURVE()
GEOMETRIC_REPRESENTATION_ITEM()
RATIONAL_B_SPLINE_CURVE((1.,1.,1.,1.,1.,1.,1.,1.,1.,1.,1.,1.,1.,1.,1.,1.,
1.,1.,1.,1.,1.,1.,1.,1.,1.,1.,1.,1.,1.,1.,1.,1.,1.,1.,1.,1.,1.,1.,1.,1.,
1.,1.,1.,1.,1.,1.,1.,1.,1.,1.,1.,1.,1.,1.,1.,1.,1.,1.,1.,1.,1.,1.,1.,1.,
1.,1.,1.,1.,1.,1.))
REPRESENTATION_ITEM('')
);
#130=(
BOUNDED_CURVE()
B_SPLINE_CURVE(5,(#32882,#32883,#32884,#32885,#32886,#32887,#32888,#32889,
#32890,#32891,#32892,#32893,#32894,#32895,#32896,#32897,#32898,#32899,#32900,
#32901,#32902,#32903,#32904,#32905,#32906,#32907,#32908,#32909,#32910,#32911,
#32912,#32913,#32914,#32915,#32916,#32917,#32918,#32919,#32920,#32921,#32922,
#32923,#32924,#32925,#32926,#32927,#32928,#32929,#32930,#32931,#32932,#32933,
#32934,#32935,#32936,#32937,#32938,#32939,#32940,#32941,#32942,#32943,#32944,
#32945,#32946,#32947,#32948,#32949,#32950,#32951),.UNSPECIFIED.,.F.,.F.)
B_SPLINE_CURVE_WITH_KNOTS((6,1,1,1,1,1,1,1,1,1,1,1,1,1,1,1,1,1,1,1,1,1,
1,1,1,1,1,1,1,1,1,1,1,1,1,1,1,1,1,1,1,1,1,1,1,1,1,1,1,1,1,1,1,1,1,1,1,1,
1,1,1,1,1,1,1,6),(-1.,-0.984615384615383,-0.969230769230768,-0.953846153846152,
-0.938461538461537,-0.923076923076922,-0.907692307692306,-0.892307692307691,
-0.876923076923076,-0.86153846153846,-0.846153846153845,-0.83076923076923,
-0.815384615384614,-0.799999999999999,-0.784615384615384,-0.769230769230768,
-0.753846153846153,-0.738461538461538,-0.723076923076922,-0.707692307692307,
-0.692307692307692,-0.676923076923076,-0.661538461538461,-0.646153846153846,
-0.63076923076923,-0.615384615384615,-0.6,-0.584615384615384,-0.569230769230769,
-0.553846153846154,-0.538461538461538,-0.523076923076923,-0.507692307692308,
-0.492307692307692,-0.476923076923077,-0.461538461538462,-0.446153846153846,
-0.430769230769231,-0.415384615384615,-0.4,-0.384615384615385,-0.369230769230769,
-0.353846153846154,-0.338461538461538,-0.323076923076923,-0.307692307692308,
-0.292307692307692,-0.276923076923077,-0.261538461538462,-0.246153846153846,
-0.230769230769231,-0.215384615384615,-0.2,-0.184615384615385,-0.169230769230769,
-0.153846153846154,-0.138461538461538,-0.123076923076923,-0.107692307692308,
-0.0923076923076923,-0.0769230769230769,-0.0615384615384615,-0.0461538461538462,
-0.0307692307692308,-0.0153846153846154,0.),.UNSPECIFIED.)
CURVE()
GEOMETRIC_REPRESENTATION_ITEM()
RATIONAL_B_SPLINE_CURVE((1.,1.,1.,1.,1.,1.,1.,1.,1.,1.,1.,1.,1.,1.,1.,1.,
1.,1.,1.,1.,1.,1.,1.,1.,1.,1.,1.,1.,1.,1.,1.,1.,1.,1.,1.,1.,1.,1.,1.,1.,
1.,1.,1.,1.,1.,1.,1.,1.,1.,1.,1.,1.,1.,1.,1.,1.,1.,1.,1.,1.,1.,1.,1.,1.,
1.,1.,1.,1.,1.,1.))
REPRESENTATION_ITEM('')
);
#131=ORIENTED_CLOSED_SHELL('',*,#12666,.F.);
#132=ORIENTED_CLOSED_SHELL('',*,#12688,.F.);
#133=ORIENTED_CLOSED_SHELL('',*,#12690,.F.);
#134=BREP_WITH_VOIDS('Body1',#12667,(#131));
#135=BREP_WITH_VOIDS('Body1',#12687,(#132));
#136=BREP_WITH_VOIDS('Body1',#12689,(#133));
#137=ITEM_DEFINED_TRANSFORMATION($,$,#13604,#13726);
#138=ITEM_DEFINED_TRANSFORMATION($,$,#13624,#13727);
#139=ITEM_DEFINED_TRANSFORMATION($,$,#13644,#13728);
#140=ITEM_DEFINED_TRANSFORMATION($,$,#13659,#13729);
#141=ITEM_DEFINED_TRANSFORMATION($,$,#13709,#13730);
#142=ITEM_DEFINED_TRANSFORMATION($,$,#13756,#13998);
#143=ITEM_DEFINED_TRANSFORMATION($,$,#13937,#13999);
#144=ITEM_DEFINED_TRANSFORMATION($,$,#13955,#14000);
#145=ITEM_DEFINED_TRANSFORMATION($,$,#13961,#14001);
#146=ITEM_DEFINED_TRANSFORMATION($,$,#13967,#14002);
#147=ITEM_DEFINED_TRANSFORMATION($,$,#13981,#14003);
#148=ITEM_DEFINED_TRANSFORMATION($,$,#13190,#14288);
#149=ITEM_DEFINED_TRANSFORMATION($,$,#13215,#14289);
#150=ITEM_DEFINED_TRANSFORMATION($,$,#13222,#14290);
#151=ITEM_DEFINED_TRANSFORMATION($,$,#13229,#14291);
#152=ITEM_DEFINED_TRANSFORMATION($,$,#13297,#14292);
#153=ITEM_DEFINED_TRANSFORMATION($,$,#13333,#14293);
#154=ITEM_DEFINED_TRANSFORMATION($,$,#13350,#14294);
#155=ITEM_DEFINED_TRANSFORMATION($,$,#13371,#14295);
#156=ITEM_DEFINED_TRANSFORMATION($,$,#13388,#14296);
#157=ITEM_DEFINED_TRANSFORMATION($,$,#13409,#14297);
#158=ITEM_DEFINED_TRANSFORMATION($,$,#13431,#14298);
#159=ITEM_DEFINED_TRANSFORMATION($,$,#13463,#14299);
#160=ITEM_DEFINED_TRANSFORMATION($,$,#13488,#14300);
#161=ITEM_DEFINED_TRANSFORMATION($,$,#13513,#14301);
#162=ITEM_DEFINED_TRANSFORMATION($,$,#13545,#14302);
#163=ITEM_DEFINED_TRANSFORMATION($,$,#13570,#14303);
#164=ITEM_DEFINED_TRANSFORMATION($,$,#13595,#14304);
#165=ITEM_DEFINED_TRANSFORMATION($,$,#13731,#14305);
#166=ITEM_DEFINED_TRANSFORMATION($,$,#13731,#14306);
#167=ITEM_DEFINED_TRANSFORMATION($,$,#13981,#14307);
#168=ITEM_DEFINED_TRANSFORMATION($,$,#13981,#14308);
#169=ITEM_DEFINED_TRANSFORMATION($,$,#13731,#14309);
#170=ITEM_DEFINED_TRANSFORMATION($,$,#13731,#14310);
#171=ITEM_DEFINED_TRANSFORMATION($,$,#13731,#14311);
#172=ITEM_DEFINED_TRANSFORMATION($,$,#13731,#14312);
#173=ITEM_DEFINED_TRANSFORMATION($,$,#13981,#14313);
#174=ITEM_DEFINED_TRANSFORMATION($,$,#14262,#14314);
#175=ITEM_DEFINED_TRANSFORMATION($,$,#14262,#14315);
#176=ITEM_DEFINED_TRANSFORMATION($,$,#13603,#14316);
#177=ITEM_DEFINED_TRANSFORMATION($,$,#13731,#14317);
#178=ITEM_DEFINED_TRANSFORMATION($,$,#13731,#14318);
#179=ITEM_DEFINED_TRANSFORMATION($,$,#13731,#14319);
#180=ITEM_DEFINED_TRANSFORMATION($,$,#13731,#14320);
#181=ITEM_DEFINED_TRANSFORMATION($,$,#13731,#14321);
#182=ITEM_DEFINED_TRANSFORMATION($,$,#13731,#14322);
#183=ITEM_DEFINED_TRANSFORMATION($,$,#13731,#14323);
#184=ITEM_DEFINED_TRANSFORMATION($,$,#13731,#14324);
#185=ITEM_DEFINED_TRANSFORMATION($,$,#14262,#14325);
#186=ITEM_DEFINED_TRANSFORMATION($,$,#14262,#14326);
#187=ITEM_DEFINED_TRANSFORMATION($,$,#13603,#14327);
#188=ITEM_DEFINED_TRANSFORMATION($,$,#13731,#14328);
#189=ITEM_DEFINED_TRANSFORMATION($,$,#13731,#14329);
#190=ITEM_DEFINED_TRANSFORMATION($,$,#13731,#14330);
#191=ITEM_DEFINED_TRANSFORMATION($,$,#13731,#14331);
#192=ITEM_DEFINED_TRANSFORMATION($,$,#13731,#14332);
#193=ITEM_DEFINED_TRANSFORMATION($,$,#13731,#14333);
#194=ITEM_DEFINED_TRANSFORMATION($,$,#13731,#14334);
#195=ITEM_DEFINED_TRANSFORMATION($,$,#13731,#14335);
#196=ITEM_DEFINED_TRANSFORMATION($,$,#14005,#14336);
#197=ITEM_DEFINED_TRANSFORMATION($,$,#14033,#14337);
#198=ITEM_DEFINED_TRANSFORMATION($,$,#14042,#14338);
#199=ITEM_DEFINED_TRANSFORMATION($,$,#14051,#14339);
#200=ITEM_DEFINED_TRANSFORMATION($,$,#14060,#14340);
#201=ITEM_DEFINED_TRANSFORMATION($,$,#14069,#14341);
#202=ITEM_DEFINED_TRANSFORMATION($,$,#14076,#14342);
#203=ITEM_DEFINED_TRANSFORMATION($,$,#14083,#14343);
#204=ITEM_DEFINED_TRANSFORMATION($,$,#14107,#14344);
#205=ITEM_DEFINED_TRANSFORMATION($,$,#14116,#14345);
#206=ITEM_DEFINED_TRANSFORMATION($,$,#14125,#14346);
#207=ITEM_DEFINED_TRANSFORMATION($,$,#14134,#14347);
#208=ITEM_DEFINED_TRANSFORMATION($,$,#14227,#14348);
#209=ITEM_DEFINED_TRANSFORMATION($,$,#14236,#14349);
#210=ITEM_DEFINED_TRANSFORMATION($,$,#14262,#14350);
#211=ITEM_DEFINED_TRANSFORMATION($,$,#14262,#14351);
#212=ITEM_DEFINED_TRANSFORMATION($,$,#14353,#14362);
#213=ITEM_DEFINED_TRANSFORMATION($,$,#13189,#14363);
#214=ITEM_DEFINED_TRANSFORMATION($,$,#13755,#14364);
#215=ITEM_DEFINED_TRANSFORMATION($,$,#14004,#14365);
#216=ITEM_DEFINED_TRANSFORMATION($,$,#14352,#14366);
#217=(
REPRESENTATION_RELATIONSHIP($,$,#33506,#33505)
REPRESENTATION_RELATIONSHIP_WITH_TRANSFORMATION(#137)
SHAPE_REPRESENTATION_RELATIONSHIP()
);
#218=(
REPRESENTATION_RELATIONSHIP($,$,#33507,#33505)
REPRESENTATION_RELATIONSHIP_WITH_TRANSFORMATION(#138)
SHAPE_REPRESENTATION_RELATIONSHIP()
);
#219=(
REPRESENTATION_RELATIONSHIP($,$,#33508,#33505)
REPRESENTATION_RELATIONSHIP_WITH_TRANSFORMATION(#139)
SHAPE_REPRESENTATION_RELATIONSHIP()
);
#220=(
REPRESENTATION_RELATIONSHIP($,$,#33509,#33505)
REPRESENTATION_RELATIONSHIP_WITH_TRANSFORMATION(#140)
SHAPE_REPRESENTATION_RELATIONSHIP()
);
#221=(
REPRESENTATION_RELATIONSHIP($,$,#33510,#33505)
REPRESENTATION_RELATIONSHIP_WITH_TRANSFORMATION(#141)
SHAPE_REPRESENTATION_RELATIONSHIP()
);
#222=(
REPRESENTATION_RELATIONSHIP($,$,#33513,#33512)
REPRESENTATION_RELATIONSHIP_WITH_TRANSFORMATION(#142)
SHAPE_REPRESENTATION_RELATIONSHIP()
);
#223=(
REPRESENTATION_RELATIONSHIP($,$,#33514,#33512)
REPRESENTATION_RELATIONSHIP_WITH_TRANSFORMATION(#143)
SHAPE_REPRESENTATION_RELATIONSHIP()
);
#224=(
REPRESENTATION_RELATIONSHIP($,$,#33515,#33512)
REPRESENTATION_RELATIONSHIP_WITH_TRANSFORMATION(#144)
SHAPE_REPRESENTATION_RELATIONSHIP()
);
#225=(
REPRESENTATION_RELATIONSHIP($,$,#33516,#33512)
REPRESENTATION_RELATIONSHIP_WITH_TRANSFORMATION(#145)
SHAPE_REPRESENTATION_RELATIONSHIP()
);
#226=(
REPRESENTATION_RELATIONSHIP($,$,#33517,#33512)
REPRESENTATION_RELATIONSHIP_WITH_TRANSFORMATION(#146)
SHAPE_REPRESENTATION_RELATIONSHIP()
);
#227=(
REPRESENTATION_RELATIONSHIP($,$,#33518,#33512)
REPRESENTATION_RELATIONSHIP_WITH_TRANSFORMATION(#147)
SHAPE_REPRESENTATION_RELATIONSHIP()
);
#228=(
REPRESENTATION_RELATIONSHIP($,$,#33488,#33487)
REPRESENTATION_RELATIONSHIP_WITH_TRANSFORMATION(#148)
SHAPE_REPRESENTATION_RELATIONSHIP()
);
#229=(
REPRESENTATION_RELATIONSHIP($,$,#33489,#33487)
REPRESENTATION_RELATIONSHIP_WITH_TRANSFORMATION(#149)
SHAPE_REPRESENTATION_RELATIONSHIP()
);
#230=(
REPRESENTATION_RELATIONSHIP($,$,#33490,#33487)
REPRESENTATION_RELATIONSHIP_WITH_TRANSFORMATION(#150)
SHAPE_REPRESENTATION_RELATIONSHIP()
);
#231=(
REPRESENTATION_RELATIONSHIP($,$,#33491,#33487)
REPRESENTATION_RELATIONSHIP_WITH_TRANSFORMATION(#151)
SHAPE_REPRESENTATION_RELATIONSHIP()
);
#232=(
REPRESENTATION_RELATIONSHIP($,$,#33492,#33487)
REPRESENTATION_RELATIONSHIP_WITH_TRANSFORMATION(#152)
SHAPE_REPRESENTATION_RELATIONSHIP()
);
#233=(
REPRESENTATION_RELATIONSHIP($,$,#33493,#33487)
REPRESENTATION_RELATIONSHIP_WITH_TRANSFORMATION(#153)
SHAPE_REPRESENTATION_RELATIONSHIP()
);
#234=(
REPRESENTATION_RELATIONSHIP($,$,#33494,#33487)
REPRESENTATION_RELATIONSHIP_WITH_TRANSFORMATION(#154)
SHAPE_REPRESENTATION_RELATIONSHIP()
);
#235=(
REPRESENTATION_RELATIONSHIP($,$,#33495,#33487)
REPRESENTATION_RELATIONSHIP_WITH_TRANSFORMATION(#155)
SHAPE_REPRESENTATION_RELATIONSHIP()
);
#236=(
REPRESENTATION_RELATIONSHIP($,$,#33496,#33487)
REPRESENTATION_RELATIONSHIP_WITH_TRANSFORMATION(#156)
SHAPE_REPRESENTATION_RELATIONSHIP()
);
#237=(
REPRESENTATION_RELATIONSHIP($,$,#33497,#33487)
REPRESENTATION_RELATIONSHIP_WITH_TRANSFORMATION(#157)
SHAPE_REPRESENTATION_RELATIONSHIP()
);
#238=(
REPRESENTATION_RELATIONSHIP($,$,#33498,#33487)
REPRESENTATION_RELATIONSHIP_WITH_TRANSFORMATION(#158)
SHAPE_REPRESENTATION_RELATIONSHIP()
);
#239=(
REPRESENTATION_RELATIONSHIP($,$,#33499,#33487)
REPRESENTATION_RELATIONSHIP_WITH_TRANSFORMATION(#159)
SHAPE_REPRESENTATION_RELATIONSHIP()
);
#240=(
REPRESENTATION_RELATIONSHIP($,$,#33500,#33487)
REPRESENTATION_RELATIONSHIP_WITH_TRANSFORMATION(#160)
SHAPE_REPRESENTATION_RELATIONSHIP()
);
#241=(
REPRESENTATION_RELATIONSHIP($,$,#33501,#33487)
REPRESENTATION_RELATIONSHIP_WITH_TRANSFORMATION(#161)
SHAPE_REPRESENTATION_RELATIONSHIP()
);
#242=(
REPRESENTATION_RELATIONSHIP($,$,#33502,#33487)
REPRESENTATION_RELATIONSHIP_WITH_TRANSFORMATION(#162)
SHAPE_REPRESENTATION_RELATIONSHIP()
);
#243=(
REPRESENTATION_RELATIONSHIP($,$,#33503,#33487)
REPRESENTATION_RELATIONSHIP_WITH_TRANSFORMATION(#163)
SHAPE_REPRESENTATION_RELATIONSHIP()
);
#244=(
REPRESENTATION_RELATIONSHIP($,$,#33504,#33487)
REPRESENTATION_RELATIONSHIP_WITH_TRANSFORMATION(#164)
SHAPE_REPRESENTATION_RELATIONSHIP()
);
#245=(
REPRESENTATION_RELATIONSHIP($,$,#33511,#33487)
REPRESENTATION_RELATIONSHIP_WITH_TRANSFORMATION(#165)
SHAPE_REPRESENTATION_RELATIONSHIP()
);
#246=(
REPRESENTATION_RELATIONSHIP($,$,#33511,#33487)
REPRESENTATION_RELATIONSHIP_WITH_TRANSFORMATION(#166)
SHAPE_REPRESENTATION_RELATIONSHIP()
);
#247=(
REPRESENTATION_RELATIONSHIP($,$,#33518,#33487)
REPRESENTATION_RELATIONSHIP_WITH_TRANSFORMATION(#167)
SHAPE_REPRESENTATION_RELATIONSHIP()
);
#248=(
REPRESENTATION_RELATIONSHIP($,$,#33518,#33487)
REPRESENTATION_RELATIONSHIP_WITH_TRANSFORMATION(#168)
SHAPE_REPRESENTATION_RELATIONSHIP()
);
#249=(
REPRESENTATION_RELATIONSHIP($,$,#33511,#33487)
REPRESENTATION_RELATIONSHIP_WITH_TRANSFORMATION(#169)
SHAPE_REPRESENTATION_RELATIONSHIP()
);
#250=(
REPRESENTATION_RELATIONSHIP($,$,#33511,#33487)
REPRESENTATION_RELATIONSHIP_WITH_TRANSFORMATION(#170)
SHAPE_REPRESENTATION_RELATIONSHIP()
);
#251=(
REPRESENTATION_RELATIONSHIP($,$,#33511,#33487)
REPRESENTATION_RELATIONSHIP_WITH_TRANSFORMATION(#171)
SHAPE_REPRESENTATION_RELATIONSHIP()
);
#252=(
REPRESENTATION_RELATIONSHIP($,$,#33511,#33487)
REPRESENTATION_RELATIONSHIP_WITH_TRANSFORMATION(#172)
SHAPE_REPRESENTATION_RELATIONSHIP()
);
#253=(
REPRESENTATION_RELATIONSHIP($,$,#33518,#33487)
REPRESENTATION_RELATIONSHIP_WITH_TRANSFORMATION(#173)
SHAPE_REPRESENTATION_RELATIONSHIP()
);
#254=(
REPRESENTATION_RELATIONSHIP($,$,#33534,#33487)
REPRESENTATION_RELATIONSHIP_WITH_TRANSFORMATION(#174)
SHAPE_REPRESENTATION_RELATIONSHIP()
);
#255=(
REPRESENTATION_RELATIONSHIP($,$,#33534,#33487)
REPRESENTATION_RELATIONSHIP_WITH_TRANSFORMATION(#175)
SHAPE_REPRESENTATION_RELATIONSHIP()
);
#256=(
REPRESENTATION_RELATIONSHIP($,$,#33505,#33487)
REPRESENTATION_RELATIONSHIP_WITH_TRANSFORMATION(#176)
SHAPE_REPRESENTATION_RELATIONSHIP()
);
#257=(
REPRESENTATION_RELATIONSHIP($,$,#33511,#33487)
REPRESENTATION_RELATIONSHIP_WITH_TRANSFORMATION(#177)
SHAPE_REPRESENTATION_RELATIONSHIP()
);
#258=(
REPRESENTATION_RELATIONSHIP($,$,#33511,#33487)
REPRESENTATION_RELATIONSHIP_WITH_TRANSFORMATION(#178)
SHAPE_REPRESENTATION_RELATIONSHIP()
);
#259=(
REPRESENTATION_RELATIONSHIP($,$,#33511,#33487)
REPRESENTATION_RELATIONSHIP_WITH_TRANSFORMATION(#179)
SHAPE_REPRESENTATION_RELATIONSHIP()
);
#260=(
REPRESENTATION_RELATIONSHIP($,$,#33511,#33487)
REPRESENTATION_RELATIONSHIP_WITH_TRANSFORMATION(#180)
SHAPE_REPRESENTATION_RELATIONSHIP()
);
#261=(
REPRESENTATION_RELATIONSHIP($,$,#33511,#33487)
REPRESENTATION_RELATIONSHIP_WITH_TRANSFORMATION(#181)
SHAPE_REPRESENTATION_RELATIONSHIP()
);
#262=(
REPRESENTATION_RELATIONSHIP($,$,#33511,#33487)
REPRESENTATION_RELATIONSHIP_WITH_TRANSFORMATION(#182)
SHAPE_REPRESENTATION_RELATIONSHIP()
);
#263=(
REPRESENTATION_RELATIONSHIP($,$,#33511,#33487)
REPRESENTATION_RELATIONSHIP_WITH_TRANSFORMATION(#183)
SHAPE_REPRESENTATION_RELATIONSHIP()
);
#264=(
REPRESENTATION_RELATIONSHIP($,$,#33511,#33487)
REPRESENTATION_RELATIONSHIP_WITH_TRANSFORMATION(#184)
SHAPE_REPRESENTATION_RELATIONSHIP()
);
#265=(
REPRESENTATION_RELATIONSHIP($,$,#33534,#33487)
REPRESENTATION_RELATIONSHIP_WITH_TRANSFORMATION(#185)
SHAPE_REPRESENTATION_RELATIONSHIP()
);
#266=(
REPRESENTATION_RELATIONSHIP($,$,#33534,#33487)
REPRESENTATION_RELATIONSHIP_WITH_TRANSFORMATION(#186)
SHAPE_REPRESENTATION_RELATIONSHIP()
);
#267=(
REPRESENTATION_RELATIONSHIP($,$,#33505,#33487)
REPRESENTATION_RELATIONSHIP_WITH_TRANSFORMATION(#187)
SHAPE_REPRESENTATION_RELATIONSHIP()
);
#268=(
REPRESENTATION_RELATIONSHIP($,$,#33511,#33487)
REPRESENTATION_RELATIONSHIP_WITH_TRANSFORMATION(#188)
SHAPE_REPRESENTATION_RELATIONSHIP()
);
#269=(
REPRESENTATION_RELATIONSHIP($,$,#33511,#33487)
REPRESENTATION_RELATIONSHIP_WITH_TRANSFORMATION(#189)
SHAPE_REPRESENTATION_RELATIONSHIP()
);
#270=(
REPRESENTATION_RELATIONSHIP($,$,#33511,#33487)
REPRESENTATION_RELATIONSHIP_WITH_TRANSFORMATION(#190)
SHAPE_REPRESENTATION_RELATIONSHIP()
);
#271=(
REPRESENTATION_RELATIONSHIP($,$,#33511,#33487)
REPRESENTATION_RELATIONSHIP_WITH_TRANSFORMATION(#191)
SHAPE_REPRESENTATION_RELATIONSHIP()
);
#272=(
REPRESENTATION_RELATIONSHIP($,$,#33511,#33487)
REPRESENTATION_RELATIONSHIP_WITH_TRANSFORMATION(#192)
SHAPE_REPRESENTATION_RELATIONSHIP()
);
#273=(
REPRESENTATION_RELATIONSHIP($,$,#33511,#33487)
REPRESENTATION_RELATIONSHIP_WITH_TRANSFORMATION(#193)
SHAPE_REPRESENTATION_RELATIONSHIP()
);
#274=(
REPRESENTATION_RELATIONSHIP($,$,#33511,#33487)
REPRESENTATION_RELATIONSHIP_WITH_TRANSFORMATION(#194)
SHAPE_REPRESENTATION_RELATIONSHIP()
);
#275=(
REPRESENTATION_RELATIONSHIP($,$,#33511,#33487)
REPRESENTATION_RELATIONSHIP_WITH_TRANSFORMATION(#195)
SHAPE_REPRESENTATION_RELATIONSHIP()
);
#276=(
REPRESENTATION_RELATIONSHIP($,$,#33520,#33519)
REPRESENTATION_RELATIONSHIP_WITH_TRANSFORMATION(#196)
SHAPE_REPRESENTATION_RELATIONSHIP()
);
#277=(
REPRESENTATION_RELATIONSHIP($,$,#33521,#33519)
REPRESENTATION_RELATIONSHIP_WITH_TRANSFORMATION(#197)
SHAPE_REPRESENTATION_RELATIONSHIP()
);
#278=(
REPRESENTATION_RELATIONSHIP($,$,#33522,#33519)
REPRESENTATION_RELATIONSHIP_WITH_TRANSFORMATION(#198)
SHAPE_REPRESENTATION_RELATIONSHIP()
);
#279=(
REPRESENTATION_RELATIONSHIP($,$,#33523,#33519)
REPRESENTATION_RELATIONSHIP_WITH_TRANSFORMATION(#199)
SHAPE_REPRESENTATION_RELATIONSHIP()
);
#280=(
REPRESENTATION_RELATIONSHIP($,$,#33524,#33519)
REPRESENTATION_RELATIONSHIP_WITH_TRANSFORMATION(#200)
SHAPE_REPRESENTATION_RELATIONSHIP()
);
#281=(
REPRESENTATION_RELATIONSHIP($,$,#33525,#33519)
REPRESENTATION_RELATIONSHIP_WITH_TRANSFORMATION(#201)
SHAPE_REPRESENTATION_RELATIONSHIP()
);
#282=(
REPRESENTATION_RELATIONSHIP($,$,#33526,#33519)
REPRESENTATION_RELATIONSHIP_WITH_TRANSFORMATION(#202)
SHAPE_REPRESENTATION_RELATIONSHIP()
);
#283=(
REPRESENTATION_RELATIONSHIP($,$,#33527,#33519)
REPRESENTATION_RELATIONSHIP_WITH_TRANSFORMATION(#203)
SHAPE_REPRESENTATION_RELATIONSHIP()
);
#284=(
REPRESENTATION_RELATIONSHIP($,$,#33528,#33519)
REPRESENTATION_RELATIONSHIP_WITH_TRANSFORMATION(#204)
SHAPE_REPRESENTATION_RELATIONSHIP()
);
#285=(
REPRESENTATION_RELATIONSHIP($,$,#33529,#33519)
REPRESENTATION_RELATIONSHIP_WITH_TRANSFORMATION(#205)
SHAPE_REPRESENTATION_RELATIONSHIP()
);
#286=(
REPRESENTATION_RELATIONSHIP($,$,#33530,#33519)
REPRESENTATION_RELATIONSHIP_WITH_TRANSFORMATION(#206)
SHAPE_REPRESENTATION_RELATIONSHIP()
);
#287=(
REPRESENTATION_RELATIONSHIP($,$,#33531,#33519)
REPRESENTATION_RELATIONSHIP_WITH_TRANSFORMATION(#207)
SHAPE_REPRESENTATION_RELATIONSHIP()
);
#288=(
REPRESENTATION_RELATIONSHIP($,$,#33532,#33519)
REPRESENTATION_RELATIONSHIP_WITH_TRANSFORMATION(#208)
SHAPE_REPRESENTATION_RELATIONSHIP()
);
#289=(
REPRESENTATION_RELATIONSHIP($,$,#33533,#33519)
REPRESENTATION_RELATIONSHIP_WITH_TRANSFORMATION(#209)
SHAPE_REPRESENTATION_RELATIONSHIP()
);
#290=(
REPRESENTATION_RELATIONSHIP($,$,#33534,#33519)
REPRESENTATION_RELATIONSHIP_WITH_TRANSFORMATION(#210)
SHAPE_REPRESENTATION_RELATIONSHIP()
);
#291=(
REPRESENTATION_RELATIONSHIP($,$,#33534,#33519)
REPRESENTATION_RELATIONSHIP_WITH_TRANSFORMATION(#211)
SHAPE_REPRESENTATION_RELATIONSHIP()
);
#292=(
REPRESENTATION_RELATIONSHIP($,$,#33536,#33535)
REPRESENTATION_RELATIONSHIP_WITH_TRANSFORMATION(#212)
SHAPE_REPRESENTATION_RELATIONSHIP()
);
#293=(
REPRESENTATION_RELATIONSHIP($,$,#33487,#33486)
REPRESENTATION_RELATIONSHIP_WITH_TRANSFORMATION(#213)
SHAPE_REPRESENTATION_RELATIONSHIP()
);
#294=(
REPRESENTATION_RELATIONSHIP($,$,#33512,#33486)
REPRESENTATION_RELATIONSHIP_WITH_TRANSFORMATION(#214)
SHAPE_REPRESENTATION_RELATIONSHIP()
);
#295=(
REPRESENTATION_RELATIONSHIP($,$,#33519,#33486)
REPRESENTATION_RELATIONSHIP_WITH_TRANSFORMATION(#215)
SHAPE_REPRESENTATION_RELATIONSHIP()
);
#296=(
REPRESENTATION_RELATIONSHIP($,$,#33535,#33486)
REPRESENTATION_RELATIONSHIP_WITH_TRANSFORMATION(#216)
SHAPE_REPRESENTATION_RELATIONSHIP()
);
#297=CONTEXT_DEPENDENT_SHAPE_REPRESENTATION(#217,#33380);
#298=CONTEXT_DEPENDENT_SHAPE_REPRESENTATION(#218,#33381);
#299=CONTEXT_DEPENDENT_SHAPE_REPRESENTATION(#219,#33382);
#300=CONTEXT_DEPENDENT_SHAPE_REPRESENTATION(#220,#33383);
#301=CONTEXT_DEPENDENT_SHAPE_REPRESENTATION(#221,#33384);
#302=CONTEXT_DEPENDENT_SHAPE_REPRESENTATION(#222,#33393);
#303=CONTEXT_DEPENDENT_SHAPE_REPRESENTATION(#223,#33394);
#304=CONTEXT_DEPENDENT_SHAPE_REPRESENTATION(#224,#33395);
#305=CONTEXT_DEPENDENT_SHAPE_REPRESENTATION(#225,#33396);
#306=CONTEXT_DEPENDENT_SHAPE_REPRESENTATION(#226,#33397);
#307=CONTEXT_DEPENDENT_SHAPE_REPRESENTATION(#227,#33398);
#308=CONTEXT_DEPENDENT_SHAPE_REPRESENTATION(#228,#33415);
#309=CONTEXT_DEPENDENT_SHAPE_REPRESENTATION(#229,#33416);
#310=CONTEXT_DEPENDENT_SHAPE_REPRESENTATION(#230,#33417);
#311=CONTEXT_DEPENDENT_SHAPE_REPRESENTATION(#231,#33418);
#312=CONTEXT_DEPENDENT_SHAPE_REPRESENTATION(#232,#33419);
#313=CONTEXT_DEPENDENT_SHAPE_REPRESENTATION(#233,#33420);
#314=CONTEXT_DEPENDENT_SHAPE_REPRESENTATION(#234,#33421);
#315=CONTEXT_DEPENDENT_SHAPE_REPRESENTATION(#235,#33422);
#316=CONTEXT_DEPENDENT_SHAPE_REPRESENTATION(#236,#33423);
#317=CONTEXT_DEPENDENT_SHAPE_REPRESENTATION(#237,#33424);
#318=CONTEXT_DEPENDENT_SHAPE_REPRESENTATION(#238,#33425);
#319=CONTEXT_DEPENDENT_SHAPE_REPRESENTATION(#239,#33426);
#320=CONTEXT_DEPENDENT_SHAPE_REPRESENTATION(#240,#33427);
#321=CONTEXT_DEPENDENT_SHAPE_REPRESENTATION(#241,#33428);
#322=CONTEXT_DEPENDENT_SHAPE_REPRESENTATION(#242,#33429);
#323=CONTEXT_DEPENDENT_SHAPE_REPRESENTATION(#243,#33430);
#324=CONTEXT_DEPENDENT_SHAPE_REPRESENTATION(#244,#33431);
#325=CONTEXT_DEPENDENT_SHAPE_REPRESENTATION(#245,#33432);
#326=CONTEXT_DEPENDENT_SHAPE_REPRESENTATION(#246,#33433);
#327=CONTEXT_DEPENDENT_SHAPE_REPRESENTATION(#247,#33434);
#328=CONTEXT_DEPENDENT_SHAPE_REPRESENTATION(#248,#33435);
#329=CONTEXT_DEPENDENT_SHAPE_REPRESENTATION(#249,#33436);
#330=CONTEXT_DEPENDENT_SHAPE_REPRESENTATION(#250,#33437);
#331=CONTEXT_DEPENDENT_SHAPE_REPRESENTATION(#251,#33438);
#332=CONTEXT_DEPENDENT_SHAPE_REPRESENTATION(#252,#33439);
#333=CONTEXT_DEPENDENT_SHAPE_REPRESENTATION(#253,#33440);
#334=CONTEXT_DEPENDENT_SHAPE_REPRESENTATION(#254,#33441);
#335=CONTEXT_DEPENDENT_SHAPE_REPRESENTATION(#255,#33442);
#336=CONTEXT_DEPENDENT_SHAPE_REPRESENTATION(#256,#33443);
#337=CONTEXT_DEPENDENT_SHAPE_REPRESENTATION(#257,#33444);
#338=CONTEXT_DEPENDENT_SHAPE_REPRESENTATION(#258,#33445);
#339=CONTEXT_DEPENDENT_SHAPE_REPRESENTATION(#259,#33446);
#340=CONTEXT_DEPENDENT_SHAPE_REPRESENTATION(#260,#33447);
#341=CONTEXT_DEPENDENT_SHAPE_REPRESENTATION(#261,#33448);
#342=CONTEXT_DEPENDENT_SHAPE_REPRESENTATION(#262,#33449);
#343=CONTEXT_DEPENDENT_SHAPE_REPRESENTATION(#263,#33450);
#344=CONTEXT_DEPENDENT_SHAPE_REPRESENTATION(#264,#33451);
#345=CONTEXT_DEPENDENT_SHAPE_REPRESENTATION(#265,#33452);
#346=CONTEXT_DEPENDENT_SHAPE_REPRESENTATION(#266,#33453);
#347=CONTEXT_DEPENDENT_SHAPE_REPRESENTATION(#267,#33454);
#348=CONTEXT_DEPENDENT_SHAPE_REPRESENTATION(#268,#33455);
#349=CONTEXT_DEPENDENT_SHAPE_REPRESENTATION(#269,#33456);
#350=CONTEXT_DEPENDENT_SHAPE_REPRESENTATION(#270,#33457);
#351=CONTEXT_DEPENDENT_SHAPE_REPRESENTATION(#271,#33458);
#352=CONTEXT_DEPENDENT_SHAPE_REPRESENTATION(#272,#33459);
#353=CONTEXT_DEPENDENT_SHAPE_REPRESENTATION(#273,#33460);
#354=CONTEXT_DEPENDENT_SHAPE_REPRESENTATION(#274,#33461);
#355=CONTEXT_DEPENDENT_SHAPE_REPRESENTATION(#275,#33462);
#356=CONTEXT_DEPENDENT_SHAPE_REPRESENTATION(#276,#33463);
#357=CONTEXT_DEPENDENT_SHAPE_REPRESENTATION(#277,#33464);
#358=CONTEXT_DEPENDENT_SHAPE_REPRESENTATION(#278,#33465);
#359=CONTEXT_DEPENDENT_SHAPE_REPRESENTATION(#279,#33466);
#360=CONTEXT_DEPENDENT_SHAPE_REPRESENTATION(#280,#33467);
#361=CONTEXT_DEPENDENT_SHAPE_REPRESENTATION(#281,#33468);
#362=CONTEXT_DEPENDENT_SHAPE_REPRESENTATION(#282,#33469);
#363=CONTEXT_DEPENDENT_SHAPE_REPRESENTATION(#283,#33470);
#364=CONTEXT_DEPENDENT_SHAPE_REPRESENTATION(#284,#33471);
#365=CONTEXT_DEPENDENT_SHAPE_REPRESENTATION(#285,#33472);
#366=CONTEXT_DEPENDENT_SHAPE_REPRESENTATION(#286,#33473);
#367=CONTEXT_DEPENDENT_SHAPE_REPRESENTATION(#287,#33474);
#368=CONTEXT_DEPENDENT_SHAPE_REPRESENTATION(#288,#33475);
#369=CONTEXT_DEPENDENT_SHAPE_REPRESENTATION(#289,#33476);
#370=CONTEXT_DEPENDENT_SHAPE_REPRESENTATION(#290,#33477);
#371=CONTEXT_DEPENDENT_SHAPE_REPRESENTATION(#291,#33478);
#372=CONTEXT_DEPENDENT_SHAPE_REPRESENTATION(#292,#33481);
#373=CONTEXT_DEPENDENT_SHAPE_REPRESENTATION(#293,#33482);
#374=CONTEXT_DEPENDENT_SHAPE_REPRESENTATION(#294,#33483);
#375=CONTEXT_DEPENDENT_SHAPE_REPRESENTATION(#295,#33484);
#376=CONTEXT_DEPENDENT_SHAPE_REPRESENTATION(#296,#33485);
#377=NEXT_ASSEMBLY_USAGE_OCCURRENCE('Inner ring:1','Inner ring:1',
'Inner ring:1',#33557,#33558,'Inner ring:1');
#378=NEXT_ASSEMBLY_USAGE_OCCURRENCE('Outer ring:1','Outer ring:1',
'Outer ring:1',#33557,#33559,'Outer ring:1');
#379=NEXT_ASSEMBLY_USAGE_OCCURRENCE('Balls:1','Balls:1','Balls:1',#33557,
#33560,'Balls:1');
#380=NEXT_ASSEMBLY_USAGE_OCCURRENCE('Cage:1','Cage:1','Cage:1',#33557,#33561,
'Cage:1');
#381=NEXT_ASSEMBLY_USAGE_OCCURRENCE('Seals 2RS:1','Seals 2RS:1',
'Seals 2RS:1',#33557,#33562,'Seals 2RS:1');
#382=NEXT_ASSEMBLY_USAGE_OCCURRENCE('Rack quill:1','Rack quill:1',
'Rack quill:1',#33564,#33565,'Rack quill:1');
#383=NEXT_ASSEMBLY_USAGE_OCCURRENCE('Tool holder:1','Tool holder:1',
'Tool holder:1',#33564,#33566,'Tool holder:1');
#384=NEXT_ASSEMBLY_USAGE_OCCURRENCE('Tool shank envelope:1',
'Tool shank envelope:1','Tool shank envelope:1',#33564,#33567,
'Tool shank envelope:1');
#385=NEXT_ASSEMBLY_USAGE_OCCURRENCE('M4 tool retaining screw:1',
'M4 tool retaining screw:1','M4 tool retaining screw:1',#33564,#33568,
'M4 tool retaining screw:1');
#386=NEXT_ASSEMBLY_USAGE_OCCURRENCE('Upper travel collar:1',
'Upper travel collar:1','Upper travel collar:1',#33564,#33569,
'Upper travel collar:1');
#387=NEXT_ASSEMBLY_USAGE_OCCURRENCE('Socket Set Screw - M4x6:5',
'Socket Set Screw - M4x6:5','Socket Set Screw - M4x6:5',#33564,#33570,
'Socket Set Screw - M4x6:5');
#388=NEXT_ASSEMBLY_USAGE_OCCURRENCE('Base:1','Base:1','Base:1',#33539,#33540,
'Base:1');
#389=NEXT_ASSEMBLY_USAGE_OCCURRENCE('Foot strip:1','Foot strip:1',
'Foot strip:1',#33539,#33541,'Foot strip:1');
#390=NEXT_ASSEMBLY_USAGE_OCCURRENCE('Foot strip (1):1',
'Foot strip (1):1','Foot strip (1):1',#33539,#33542,'Foot strip (1):1');
#391=NEXT_ASSEMBLY_USAGE_OCCURRENCE('Head frame:1','Head frame:1',
'Head frame:1',#33539,#33543,'Head frame:1');
#392=NEXT_ASSEMBLY_USAGE_OCCURRENCE('Column socket:1','Column socket:1',
'Column socket:1',#33539,#33544,'Column socket:1');
#393=NEXT_ASSEMBLY_USAGE_OCCURRENCE('Split ram guide:1',
'Split ram guide:1','Split ram guide:1',#33539,#33545,
'Split ram guide:1');
#394=NEXT_ASSEMBLY_USAGE_OCCURRENCE('Guide keeper:1','Guide keeper:1',
'Guide keeper:1',#33539,#33546,'Guide keeper:1');
#395=NEXT_ASSEMBLY_USAGE_OCCURRENCE('Split ram guide (1):1',
'Split ram guide (1):1','Split ram guide (1):1',#33539,#33547,
'Split ram guide (1):1');
#396=NEXT_ASSEMBLY_USAGE_OCCURRENCE('Guide keeper (1):1',
'Guide keeper (1):1','Guide keeper (1):1',#33539,#33548,
'Guide keeper (1):1');
#397=NEXT_ASSEMBLY_USAGE_OCCURRENCE('Adjustable worktable:1',
'Adjustable worktable:1','Adjustable worktable:1',#33539,#33549,
'Adjustable worktable:1');
#398=NEXT_ASSEMBLY_USAGE_OCCURRENCE('Pinion bearing pedestal:1',
'Pinion bearing pedestal:1','Pinion bearing pedestal:1',#33539,#33550,
'Pinion bearing pedestal:1');
#399=NEXT_ASSEMBLY_USAGE_OCCURRENCE('Pinion bearing cap:1',
'Pinion bearing cap:1','Pinion bearing cap:1',#33539,#33551,
'Pinion bearing cap:1');
#400=NEXT_ASSEMBLY_USAGE_OCCURRENCE('Pinion bearing cap (1):1',
'Pinion bearing cap (1):1','Pinion bearing cap (1):1',#33539,#33552,
'Pinion bearing cap (1):1');
#401=NEXT_ASSEMBLY_USAGE_OCCURRENCE('Pinion bearing pedestal (1):1',
'Pinion bearing pedestal (1):1','Pinion bearing pedestal (1):1',#33539,
#33553,'Pinion bearing pedestal (1):1');
#402=NEXT_ASSEMBLY_USAGE_OCCURRENCE('Pinion bearing cap (2):1',
'Pinion bearing cap (2):1','Pinion bearing cap (2):1',#33539,#33554,
'Pinion bearing cap (2):1');
#403=NEXT_ASSEMBLY_USAGE_OCCURRENCE('Pinion bearing cap (3):1',
'Pinion bearing cap (3):1','Pinion bearing cap (3):1',#33539,#33555,
'Pinion bearing cap (3):1');
#404=NEXT_ASSEMBLY_USAGE_OCCURRENCE('Column shaft 120 mm:2',
'Column shaft 120 mm:2','Column shaft 120 mm:2',#33539,#33556,
'Column shaft 120 mm:2');
#405=NEXT_ASSEMBLY_USAGE_OCCURRENCE('M4x10 Cap Screw:2',
'M4x10 Cap Screw:2','M4x10 Cap Screw:2',#33539,#33563,
'M4x10 Cap Screw:2');
#406=NEXT_ASSEMBLY_USAGE_OCCURRENCE('M4x10 Cap Screw:3',
'M4x10 Cap Screw:3','M4x10 Cap Screw:3',#33539,#33563,
'M4x10 Cap Screw:3');
#407=NEXT_ASSEMBLY_USAGE_OCCURRENCE('Socket Set Screw - M4x6:2',
'Socket Set Screw - M4x6:2','Socket Set Screw - M4x6:2',#33539,#33570,
'Socket Set Screw - M4x6:2');
#408=NEXT_ASSEMBLY_USAGE_OCCURRENCE('Socket Set Screw - M4x6:3',
'Socket Set Screw - M4x6:3','Socket Set Screw - M4x6:3',#33539,#33570,
'Socket Set Screw - M4x6:3');
#409=NEXT_ASSEMBLY_USAGE_OCCURRENCE('M4x10 Cap Screw:4',
'M4x10 Cap Screw:4','M4x10 Cap Screw:4',#33539,#33563,
'M4x10 Cap Screw:4');
#410=NEXT_ASSEMBLY_USAGE_OCCURRENCE('M4x10 Cap Screw:5',
'M4x10 Cap Screw:5','M4x10 Cap Screw:5',#33539,#33563,
'M4x10 Cap Screw:5');
#411=NEXT_ASSEMBLY_USAGE_OCCURRENCE('M4x10 Cap Screw:6',
'M4x10 Cap Screw:6','M4x10 Cap Screw:6',#33539,#33563,
'M4x10 Cap Screw:6');
#412=NEXT_ASSEMBLY_USAGE_OCCURRENCE('M4x10 Cap Screw:7',
'M4x10 Cap Screw:7','M4x10 Cap Screw:7',#33539,#33563,
'M4x10 Cap Screw:7');
#413=NEXT_ASSEMBLY_USAGE_OCCURRENCE('Socket Set Screw - M4x6:4',
'Socket Set Screw - M4x6:4','Socket Set Screw - M4x6:4',#33539,#33570,
'Socket Set Screw - M4x6:4');
#414=NEXT_ASSEMBLY_USAGE_OCCURRENCE('Cap Screw - M4x16:2',
'Cap Screw - M4x16:2','Cap Screw - M4x16:2',#33539,#33586,
'Cap Screw - M4x16:2');
#415=NEXT_ASSEMBLY_USAGE_OCCURRENCE('Cap Screw - M4x16:3',
'Cap Screw - M4x16:3','Cap Screw - M4x16:3',#33539,#33586,
'Cap Screw - M4x16:3');
#416=NEXT_ASSEMBLY_USAGE_OCCURRENCE(
'Sealed Ball Bearing - 12 x 32 x 10 mm:2',
'Sealed Ball Bearing - 12 x 32 x 10 mm:2',
'Sealed Ball Bearing - 12 x 32 x 10 mm:2',#33539,#33557,
'Sealed Ball Bearing - 12 x 32 x 10 mm:2');
#417=NEXT_ASSEMBLY_USAGE_OCCURRENCE('M4x10 Cap Screw:8',
'M4x10 Cap Screw:8','M4x10 Cap Screw:8',#33539,#33563,
'M4x10 Cap Screw:8');
#418=NEXT_ASSEMBLY_USAGE_OCCURRENCE('M4x10 Cap Screw:9',
'M4x10 Cap Screw:9','M4x10 Cap Screw:9',#33539,#33563,
'M4x10 Cap Screw:9');
#419=NEXT_ASSEMBLY_USAGE_OCCURRENCE('M4x10 Cap Screw:10',
'M4x10 Cap Screw:10','M4x10 Cap Screw:10',#33539,#33563,
'M4x10 Cap Screw:10');
#420=NEXT_ASSEMBLY_USAGE_OCCURRENCE('M4x10 Cap Screw:11',
'M4x10 Cap Screw:11','M4x10 Cap Screw:11',#33539,#33563,
'M4x10 Cap Screw:11');
#421=NEXT_ASSEMBLY_USAGE_OCCURRENCE('M4x10 Cap Screw:12',
'M4x10 Cap Screw:12','M4x10 Cap Screw:12',#33539,#33563,
'M4x10 Cap Screw:12');
#422=NEXT_ASSEMBLY_USAGE_OCCURRENCE('M4x10 Cap Screw:13',
'M4x10 Cap Screw:13','M4x10 Cap Screw:13',#33539,#33563,
'M4x10 Cap Screw:13');
#423=NEXT_ASSEMBLY_USAGE_OCCURRENCE('M4x10 Cap Screw:14',
'M4x10 Cap Screw:14','M4x10 Cap Screw:14',#33539,#33563,
'M4x10 Cap Screw:14');
#424=NEXT_ASSEMBLY_USAGE_OCCURRENCE('M4x10 Cap Screw:15',
'M4x10 Cap Screw:15','M4x10 Cap Screw:15',#33539,#33563,
'M4x10 Cap Screw:15');
#425=NEXT_ASSEMBLY_USAGE_OCCURRENCE('Cap Screw - M4x16:4',
'Cap Screw - M4x16:4','Cap Screw - M4x16:4',#33539,#33586,
'Cap Screw - M4x16:4');
#426=NEXT_ASSEMBLY_USAGE_OCCURRENCE('Cap Screw - M4x16:5',
'Cap Screw - M4x16:5','Cap Screw - M4x16:5',#33539,#33586,
'Cap Screw - M4x16:5');
#427=NEXT_ASSEMBLY_USAGE_OCCURRENCE(
'Sealed Ball Bearing - 12 x 32 x 10 mm:3',
'Sealed Ball Bearing - 12 x 32 x 10 mm:3',
'Sealed Ball Bearing - 12 x 32 x 10 mm:3',#33539,#33557,
'Sealed Ball Bearing - 12 x 32 x 10 mm:3');
#428=NEXT_ASSEMBLY_USAGE_OCCURRENCE('M4x10 Cap Screw:16',
'M4x10 Cap Screw:16','M4x10 Cap Screw:16',#33539,#33563,
'M4x10 Cap Screw:16');
#429=NEXT_ASSEMBLY_USAGE_OCCURRENCE('M4x10 Cap Screw:17',
'M4x10 Cap Screw:17','M4x10 Cap Screw:17',#33539,#33563,
'M4x10 Cap Screw:17');
#430=NEXT_ASSEMBLY_USAGE_OCCURRENCE('M4x10 Cap Screw:18',
'M4x10 Cap Screw:18','M4x10 Cap Screw:18',#33539,#33563,
'M4x10 Cap Screw:18');
#431=NEXT_ASSEMBLY_USAGE_OCCURRENCE('M4x10 Cap Screw:19',
'M4x10 Cap Screw:19','M4x10 Cap Screw:19',#33539,#33563,
'M4x10 Cap Screw:19');
#432=NEXT_ASSEMBLY_USAGE_OCCURRENCE('M4x10 Cap Screw:20',
'M4x10 Cap Screw:20','M4x10 Cap Screw:20',#33539,#33563,
'M4x10 Cap Screw:20');
#433=NEXT_ASSEMBLY_USAGE_OCCURRENCE('M4x10 Cap Screw:21',
'M4x10 Cap Screw:21','M4x10 Cap Screw:21',#33539,#33563,
'M4x10 Cap Screw:21');
#434=NEXT_ASSEMBLY_USAGE_OCCURRENCE('M4x10 Cap Screw:22',
'M4x10 Cap Screw:22','M4x10 Cap Screw:22',#33539,#33563,
'M4x10 Cap Screw:22');
#435=NEXT_ASSEMBLY_USAGE_OCCURRENCE('M4x10 Cap Screw:23',
'M4x10 Cap Screw:23','M4x10 Cap Screw:23',#33539,#33563,
'M4x10 Cap Screw:23');
#436=NEXT_ASSEMBLY_USAGE_OCCURRENCE('Pinion shaft:1','Pinion shaft:1',
'Pinion shaft:1',#33571,#33572,'Pinion shaft:1');
#437=NEXT_ASSEMBLY_USAGE_OCCURRENCE('Inner race spacer 20 mm:1',
'Inner race spacer 20 mm:1','Inner race spacer 20 mm:1',#33571,#33573,
'Inner race spacer 20 mm:1');
#438=NEXT_ASSEMBLY_USAGE_OCCURRENCE('Inner race spacer 15 mm:1',
'Inner race spacer 15 mm:1','Inner race spacer 15 mm:1',#33571,#33574,
'Inner race spacer 15 mm:1');
#439=NEXT_ASSEMBLY_USAGE_OCCURRENCE('Inner race spacer 3 mm:1',
'Inner race spacer 3 mm:1','Inner race spacer 3 mm:1',#33571,#33575,
'Inner race spacer 3 mm:1');
#440=NEXT_ASSEMBLY_USAGE_OCCURRENCE('Inner race spacer 15 mm (1):1',
'Inner race spacer 15 mm (1):1','Inner race spacer 15 mm (1):1',#33571,
#33576,'Inner race spacer 15 mm (1):1');
#441=NEXT_ASSEMBLY_USAGE_OCCURRENCE('Parallel key 4 x 4 x 14 mm:1',
'Parallel key 4 x 4 x 14 mm:1','Parallel key 4 x 4 x 14 mm:1',#33571,#33577,
'Parallel key 4 x 4 x 14 mm:1');
#442=NEXT_ASSEMBLY_USAGE_OCCURRENCE('Parallel key 4 x 4 x 14 mm (1):1',
'Parallel key 4 x 4 x 14 mm (1):1','Parallel key 4 x 4 x 14 mm (1):1',#33571,
#33578,'Parallel key 4 x 4 x 14 mm (1):1');
#443=NEXT_ASSEMBLY_USAGE_OCCURRENCE('Operating lever:1',
'Operating lever:1','Operating lever:1',#33571,#33579,
'Operating lever:1');
#444=NEXT_ASSEMBLY_USAGE_OCCURRENCE('Handle sleeve:1','Handle sleeve:1',
'Handle sleeve:1',#33571,#33580,'Handle sleeve:1');
#445=NEXT_ASSEMBLY_USAGE_OCCURRENCE('Shaft keeper:1','Shaft keeper:1',
'Shaft keeper:1',#33571,#33581,'Shaft keeper:1');
#446=NEXT_ASSEMBLY_USAGE_OCCURRENCE('Shaft keeper (1):1',
'Shaft keeper (1):1','Shaft keeper (1):1',#33571,#33582,
'Shaft keeper (1):1');
#447=NEXT_ASSEMBLY_USAGE_OCCURRENCE(
'Spur Gear - Module 2, 20 Teeth, 12 mm Bore:2',
'Spur Gear - Module 2, 20 Teeth, 12 mm Bore:2',
'Spur Gear - Module 2, 20 Teeth, 12 mm Bore:2',#33571,#33583,
'Spur Gear - Module 2, 20 Teeth, 12 mm Bore:2');
#448=NEXT_ASSEMBLY_USAGE_OCCURRENCE('Flat Washer - M6:2',
'Flat Washer - M6:2','Flat Washer - M6:2',#33571,#33584,
'Flat Washer - M6:2');
#449=NEXT_ASSEMBLY_USAGE_OCCURRENCE('Cap Screw - M6x25:2',
'Cap Screw - M6x25:2','Cap Screw - M6x25:2',#33571,#33585,
'Cap Screw - M6x25:2');
#450=NEXT_ASSEMBLY_USAGE_OCCURRENCE('Cap Screw - M4x16:6',
'Cap Screw - M4x16:6','Cap Screw - M4x16:6',#33571,#33586,
'Cap Screw - M4x16:6');
#451=NEXT_ASSEMBLY_USAGE_OCCURRENCE('Cap Screw - M4x16:7',
'Cap Screw - M4x16:7','Cap Screw - M4x16:7',#33571,#33586,
'Cap Screw - M4x16:7');
#452=NEXT_ASSEMBLY_USAGE_OCCURRENCE('Revolving grip:1',
'Revolving grip:1','Revolving grip:1',#33587,#33588,'Revolving grip:1');
#453=NEXT_ASSEMBLY_USAGE_OCCURRENCE('Column, head and worktable:1',
'Column, head and worktable:1','Column, head and worktable:1',#33538,#33539,
'Column, head and worktable:1');
#454=NEXT_ASSEMBLY_USAGE_OCCURRENCE('Rack quill and tool holder:1',
'Rack quill and tool holder:1','Rack quill and tool holder:1',#33538,#33564,
'Rack quill and tool holder:1');
#455=NEXT_ASSEMBLY_USAGE_OCCURRENCE('Pinion and operating lever:1',
'Pinion and operating lever:1','Pinion and operating lever:1',#33538,#33571,
'Pinion and operating lever:1');
#456=NEXT_ASSEMBLY_USAGE_OCCURRENCE('Revolving hand grip:1',
'Revolving hand grip:1','Revolving hand grip:1',#33538,#33587,
'Revolving hand grip:1');
#457=SPHERICAL_SURFACE('',#13645,0.29765);
#458=SPHERICAL_SURFACE('',#13647,0.29765);
#459=SPHERICAL_SURFACE('',#13649,0.29765);
#460=SPHERICAL_SURFACE('',#13651,0.29765);
#461=SPHERICAL_SURFACE('',#13653,0.29765);
#462=SPHERICAL_SURFACE('',#13655,0.29765);
#463=SPHERICAL_SURFACE('',#13657,0.29765);
#464=SPHERICAL_SURFACE('',#13660,0.309556);
#465=SPHERICAL_SURFACE('',#13676,0.309556);
#466=SPHERICAL_SURFACE('',#13681,0.309556);
#467=SPHERICAL_SURFACE('',#13687,0.309556);
#468=SPHERICAL_SURFACE('',#13692,0.309556);
#469=SPHERICAL_SURFACE('',#13697,0.309556);
#470=SPHERICAL_SURFACE('',#13705,0.309556);
#471=TOROIDAL_SURFACE('',#13605,1.1,0.309556);
#472=TOROIDAL_SURFACE('',#13625,1.1,0.309556);
#473=CONICAL_SURFACE('',#13598,0.55,0.785398163397448);
#474=CONICAL_SURFACE('',#13616,0.63,0.785398163397448);
#475=CONICAL_SURFACE('',#13623,0.63,0.785398163397448);
#476=CONICAL_SURFACE('',#13636,1.57,0.785398163397449);
#477=CONICAL_SURFACE('',#13640,1.57,0.785398163397449);
#478=CONICAL_SURFACE('',#13744,0.325,0.785398163397448);
#479=CONICAL_SURFACE('',#13748,0.335,0.785398163397448);
#480=CONICAL_SURFACE('',#13752,0.21,0.463647609000806);
#481=CONICAL_SURFACE('',#13991,0.185,0.785398163397449);
#482=CONICAL_SURFACE('',#13995,0.1625,0.785398163397449);
#483=CONICAL_SURFACE('',#14239,0.475,0.785398163397449);
#484=CONICAL_SURFACE('',#14243,0.485,0.785398163397448);
#485=CONICAL_SURFACE('',#14247,0.31,0.463647609000806);
#486=CONICAL_SURFACE('',#14251,0.27,0.785398163397448);
#487=CONICAL_SURFACE('',#14265,0.325,0.785398163397448);
#488=CONICAL_SURFACE('',#14269,0.335,0.785398163397448);
#489=CONICAL_SURFACE('',#14273,0.21,0.463647609000806);
#490=CONICAL_SURFACE('',#14277,0.18,0.785398163397448);
#491=B_SPLINE_CURVE_WITH_KNOTS('',3,(#18163,#18164,#18165,#18166,#18167,
#18168,#18169,#18170,#18171,#18172,#18173,#18174,#18175,#18176),
 .UNSPECIFIED.,.F.,.F.,(4,2,2,2,2,2,4),(0.598759573717645,0.624973342427789,
0.687463163426141,0.749952984424493,0.812442805422845,0.874932626421197,
0.901146395131337),.UNSPECIFIED.);
#492=B_SPLINE_CURVE_WITH_KNOTS('',3,(#18180,#18181,#18182,#18183,#18184,
#18185,#18186,#18187),.UNSPECIFIED.,.F.,.F.,(4,2,2,4),(0.249984328141498,
0.31247414913985,0.374963970138202,0.401177738848345),.UNSPECIFIED.);
#493=B_SPLINE_CURVE_WITH_KNOTS('',3,(#18191,#18192,#18193,#18194,#18195,
#18196,#18197,#18198,#18199,#18200,#18201,#18202,#18203,#18204,#18205,#18206,
#18207,#18208,#18209,#18210,#18211,#18212,#18213,#18214,#18215,#18216),
 .UNSPECIFIED.,.F.,.F.,(4,2,2,2,2,2,2,2,2,2,2,2,4),(0.,0.0622156192199746,
0.124431238439949,0.186646447577113,0.248861656714277,0.31107686585144,
0.373292074988604,0.435507694208579,0.497723313428553,0.559938932648528,
0.622154551868502,0.684369761005666,0.74658497014283),.UNSPECIFIED.);
#494=B_SPLINE_CURVE_WITH_KNOTS('',3,(#18217,#18218,#18219,#18220,#18221,
#18222,#18223,#18224,#18225,#18226),.UNSPECIFIED.,.F.,.F.,(4,2,2,2,4),(0.74658497014283,
0.808800179279993,0.871015388417157,0.933231007637132,0.995446626857106),
 .UNSPECIFIED.);
#495=B_SPLINE_CURVE_WITH_KNOTS('',3,(#18227,#18228,#18229,#18230,#18231,
#18232,#18233,#18234),.UNSPECIFIED.,.F.,.F.,(4,2,2,4),(0.098790917434652,
0.125004686144793,0.187494507143146,0.249984328141498),.UNSPECIFIED.);
#496=B_SPLINE_CURVE_WITH_KNOTS('',3,(#18304,#18305,#18306,#18307,#18308,
#18309,#18310,#18311,#18312,#18313,#18314,#18315,#18316,#18317),
 .UNSPECIFIED.,.F.,.F.,(4,2,2,2,2,2,4),(0.598759573717651,0.624973342427791,
0.687463163426144,0.749952984424497,0.812442805422849,0.874932626421202,
0.901146395131342),.UNSPECIFIED.);
#497=B_SPLINE_CURVE_WITH_KNOTS('',3,(#18321,#18322,#18323,#18324,#18325,
#18326,#18327,#18328),.UNSPECIFIED.,.F.,.F.,(4,2,2,4),(0.249984328141499,
0.312474149139851,0.374963970138204,0.401177738848344),.UNSPECIFIED.);
#498=B_SPLINE_CURVE_WITH_KNOTS('',3,(#18332,#18333,#18334,#18335,#18336,
#18337,#18338,#18339,#18340,#18341,#18342,#18343,#18344,#18345,#18346,#18347,
#18348,#18349,#18350,#18351,#18352,#18353,#18354,#18355,#18356,#18357),
 .UNSPECIFIED.,.F.,.F.,(4,2,2,2,2,2,2,2,2,2,2,2,4),(0.,0.0622156192199746,
0.124431238439949,0.186646447577113,0.248861656714278,0.311076865851442,
0.373292074988606,0.43550769420858,0.497723313428555,0.55993893264853,0.622154551868504,
0.684369761005668,0.746584970142833),.UNSPECIFIED.);
#499=B_SPLINE_CURVE_WITH_KNOTS('',3,(#18358,#18359,#18360,#18361,#18362,
#18363,#18364,#18365,#18366,#18367),.UNSPECIFIED.,.F.,.F.,(4,2,2,2,4),(0.746584970142833,
0.808800179279997,0.871015388417161,0.933231007637136,0.99544662685711),
 .UNSPECIFIED.);
#500=B_SPLINE_CURVE_WITH_KNOTS('',3,(#18368,#18369,#18370,#18371,#18372,
#18373,#18374,#18375),.UNSPECIFIED.,.F.,.F.,(4,2,2,4),(0.0987909174346533,
0.125004686144794,0.187494507143146,0.249984328141499),.UNSPECIFIED.);
#501=B_SPLINE_CURVE_WITH_KNOTS('',3,(#18696,#18697,#18698,#18699,#18700,
#18701,#18702,#18703,#18704,#18705,#18706,#18707,#18708,#18709),
 .UNSPECIFIED.,.F.,.F.,(4,2,2,2,2,2,4),(0.598759573717651,0.624973342427791,
0.687463163426144,0.749952984424497,0.812442805422849,0.874932626421202,
0.901146395131343),.UNSPECIFIED.);
#502=B_SPLINE_CURVE_WITH_KNOTS('',3,(#18713,#18714,#18715,#18716,#18717,
#18718,#18719,#18720),.UNSPECIFIED.,.F.,.F.,(4,2,2,4),(0.249984328141499,
0.312474149139851,0.374963970138204,0.401177738848344),.UNSPECIFIED.);
#503=B_SPLINE_CURVE_WITH_KNOTS('',3,(#18724,#18725,#18726,#18727,#18728,
#18729,#18730,#18731,#18732,#18733,#18734,#18735,#18736,#18737,#18738,#18739,
#18740,#18741,#18742,#18743,#18744,#18745,#18746,#18747,#18748,#18749),
 .UNSPECIFIED.,.F.,.F.,(4,2,2,2,2,2,2,2,2,2,2,2,4),(0.,0.0622156192199746,
0.124431238439949,0.186646447577113,0.248861656714278,0.311076865851442,
0.373292074988606,0.43550769420858,0.497723313428555,0.55993893264853,0.622154551868504,
0.684369761005668,0.746584970142833),.UNSPECIFIED.);
#504=B_SPLINE_CURVE_WITH_KNOTS('',3,(#18750,#18751,#18752,#18753,#18754,
#18755,#18756,#18757,#18758,#18759),.UNSPECIFIED.,.F.,.F.,(4,2,2,2,4),(0.746584970142833,
0.808800179279997,0.871015388417161,0.933231007637136,0.99544662685711),
 .UNSPECIFIED.);
#505=B_SPLINE_CURVE_WITH_KNOTS('',3,(#18760,#18761,#18762,#18763,#18764,
#18765,#18766,#18767),.UNSPECIFIED.,.F.,.F.,(4,2,2,4),(0.0987909174346536,
0.125004686144794,0.187494507143146,0.249984328141499),.UNSPECIFIED.);
#506=B_SPLINE_CURVE_WITH_KNOTS('',3,(#19268,#19269,#19270,#19271,#19272,
#19273,#19274,#19275,#19276,#19277,#19278,#19279,#19280,#19281,#19282,#19283,
#19284,#19285,#19286,#19287,#19288,#19289),.UNSPECIFIED.,.F.,.F.,(4,2,2,
2,2,2,2,2,2,2,4),(0.0591825211272536,0.157966726598481,0.236950089897721,
0.315933453196962,0.391576304923761,0.46721915665056,0.54286200837736,0.618504860104159,
0.697488223403399,0.77647158670264,0.875255792173867),.UNSPECIFIED.);
#507=B_SPLINE_CURVE_WITH_KNOTS('',3,(#19293,#19294,#19295,#19296,#19297,
#19298,#19299,#19300,#19301,#19302,#19303,#19304,#19305,#19306,#19307,#19308,
#19309,#19310,#19311,#19312,#19313,#19314),.UNSPECIFIED.,.F.,.F.,(4,2,2,
2,2,2,2,2,2,2,4),(0.0581119756758434,0.106553146291161,0.213106292582322,
0.30849933801665,0.386091982889075,0.4636846277615,0.541277272633925,0.61886991750635,
0.714262962940678,0.820816109231839,0.869257279847157),.UNSPECIFIED.);
#508=B_SPLINE_CURVE_WITH_KNOTS('',3,(#19320,#19321,#19322,#19323,#19324,
#19325,#19326,#19327,#19328,#19329,#19330,#19331,#19332,#19333,#19334,#19335,
#19336,#19337,#19338,#19339,#19340,#19341),.UNSPECIFIED.,.F.,.F.,(4,2,2,
2,2,2,2,2,2,2,4),(0.0581119756758434,0.106553146291161,0.213106292582322,
0.30849933801665,0.386091982889075,0.4636846277615,0.541277272633925,0.61886991750635,
0.714262962940679,0.820816109231839,0.869257279847157),.UNSPECIFIED.);
#509=B_SPLINE_CURVE_WITH_KNOTS('',3,(#19345,#19346,#19347,#19348,#19349,
#19350,#19351,#19352,#19353,#19354,#19355,#19356,#19357,#19358,#19359,#19360,
#19361,#19362,#19363,#19364,#19365,#19366),.UNSPECIFIED.,.F.,.F.,(4,2,2,
2,2,2,2,2,2,2,4),(0.0581119756758433,0.106553146291161,0.213106292582322,
0.308499338016649,0.386091982889075,0.4636846277615,0.541277272633925,0.61886991750635,
0.714262962940678,0.820816109231839,0.869257279847157),.UNSPECIFIED.);
#510=B_SPLINE_CURVE_WITH_KNOTS('',3,(#19375,#19376,#19377,#19378,#19379,
#19380,#19381,#19382,#19383,#19384,#19385,#19386,#19387,#19388,#19389,#19390,
#19391,#19392,#19393,#19394,#19395,#19396),.UNSPECIFIED.,.F.,.F.,(4,2,2,
2,2,2,2,2,2,2,4),(0.0581119756758433,0.106553146291161,0.213106292582322,
0.30849933801665,0.386091982889075,0.4636846277615,0.541277272633925,0.61886991750635,
0.714262962940678,0.820816109231839,0.869257279847157),.UNSPECIFIED.);
#511=B_SPLINE_CURVE_WITH_KNOTS('',3,(#19400,#19401,#19402,#19403,#19404,
#19405,#19406,#19407,#19408,#19409,#19410,#19411,#19412,#19413,#19414,#19415,
#19416,#19417,#19418,#19419,#19420,#19421),.UNSPECIFIED.,.F.,.F.,(4,2,2,
2,2,2,2,2,2,2,4),(0.0581119756758434,0.106553146291161,0.213106292582322,
0.30849933801665,0.386091982889075,0.4636846277615,0.541277272633925,0.61886991750635,
0.714262962940678,0.820816109231839,0.869257279847157),.UNSPECIFIED.);
#512=B_SPLINE_CURVE_WITH_KNOTS('',3,(#19425,#19426,#19427,#19428,#19429,
#19430,#19431,#19432,#19433,#19434,#19435,#19436,#19437,#19438,#19439,#19440,
#19441,#19442,#19443,#19444,#19445,#19446),.UNSPECIFIED.,.F.,.F.,(4,2,2,
2,2,2,2,2,2,2,4),(0.0581119756758434,0.106553146291161,0.213106292582322,
0.30849933801665,0.386091982889075,0.4636846277615,0.541277272633925,0.61886991750635,
0.714262962940678,0.820816109231839,0.869257279847157),.UNSPECIFIED.);
#513=B_SPLINE_CURVE_WITH_KNOTS('',3,(#19450,#19451,#19452,#19453,#19454,
#19455,#19456,#19457,#19458,#19459,#19460,#19461,#19462,#19463,#19464,#19465,
#19466,#19467,#19468,#19469,#19470,#19471),.UNSPECIFIED.,.F.,.F.,(4,2,2,
2,2,2,2,2,2,2,4),(0.0581119756758433,0.106553146291161,0.213106292582322,
0.30849933801665,0.386091982889075,0.4636846277615,0.541277272633925,0.61886991750635,
0.714262962940678,0.820816109231839,0.869257279847157),.UNSPECIFIED.);
#514=B_SPLINE_CURVE_WITH_KNOTS('',3,(#19479,#19480,#19481,#19482,#19483,
#19484,#19485,#19486,#19487,#19488,#19489,#19490,#19491,#19492,#19493,#19494,
#19495,#19496,#19497,#19498,#19499,#19500),.UNSPECIFIED.,.F.,.F.,(4,2,2,
2,2,2,2,2,2,2,4),(0.0591825211272536,0.157966726598481,0.236950089897721,
0.315933453196962,0.391576304923761,0.467219156650561,0.54286200837736,
0.618504860104159,0.697488223403399,0.77647158670264,0.875255792173867),
 .UNSPECIFIED.);
#515=B_SPLINE_CURVE_WITH_KNOTS('',3,(#19508,#19509,#19510,#19511,#19512,
#19513,#19514,#19515,#19516,#19517,#19518,#19519,#19520,#19521,#19522,#19523,
#19524,#19525,#19526,#19527,#19528,#19529),.UNSPECIFIED.,.F.,.F.,(4,2,2,
2,2,2,2,2,2,2,4),(0.0591825211272536,0.157966726598481,0.236950089897722,
0.315933453196962,0.391576304923761,0.467219156650561,0.54286200837736,
0.618504860104159,0.697488223403399,0.77647158670264,0.875255792173867),
 .UNSPECIFIED.);
#516=B_SPLINE_CURVE_WITH_KNOTS('',3,(#19539,#19540,#19541,#19542,#19543,
#19544,#19545,#19546,#19547,#19548,#19549,#19550,#19551,#19552,#19553,#19554,
#19555,#19556,#19557,#19558,#19559,#19560),.UNSPECIFIED.,.F.,.F.,(4,2,2,
2,2,2,2,2,2,2,4),(0.0591825211272536,0.157966726598481,0.236950089897721,
0.315933453196962,0.391576304923761,0.46721915665056,0.54286200837736,0.618504860104159,
0.697488223403399,0.77647158670264,0.875255792173867),.UNSPECIFIED.);
#517=B_SPLINE_CURVE_WITH_KNOTS('',3,(#19568,#19569,#19570,#19571,#19572,
#19573,#19574,#19575,#19576,#19577,#19578,#19579,#19580,#19581,#19582,#19583,
#19584,#19585,#19586,#19587,#19588,#19589),.UNSPECIFIED.,.F.,.F.,(4,2,2,
2,2,2,2,2,2,2,4),(0.0591825211272536,0.157966726598481,0.236950089897721,
0.315933453196962,0.391576304923761,0.46721915665056,0.542862008377359,
0.618504860104159,0.697488223403399,0.776471586702639,0.875255792173867),
 .UNSPECIFIED.);
#518=B_SPLINE_CURVE_WITH_KNOTS('',3,(#19597,#19598,#19599,#19600,#19601,
#19602,#19603,#19604,#19605,#19606,#19607,#19608,#19609,#19610,#19611,#19612,
#19613,#19614,#19615,#19616,#19617,#19618),.UNSPECIFIED.,.F.,.F.,(4,2,2,
2,2,2,2,2,2,2,4),(0.0591825211272536,0.157966726598481,0.236950089897721,
0.315933453196962,0.391576304923761,0.46721915665056,0.54286200837736,0.618504860104159,
0.697488223403399,0.77647158670264,0.875255792173867),.UNSPECIFIED.);
#519=B_SPLINE_CURVE_WITH_KNOTS('',3,(#19627,#19628,#19629,#19630,#19631,
#19632,#19633,#19634,#19635,#19636,#19637,#19638,#19639,#19640,#19641,#19642,
#19643,#19644,#19645,#19646,#19647,#19648),.UNSPECIFIED.,.F.,.F.,(4,2,2,
2,2,2,2,2,2,2,4),(0.0591825211272536,0.157966726598481,0.236950089897721,
0.315933453196962,0.391576304923761,0.46721915665056,0.542862008377359,
0.618504860104159,0.697488223403399,0.776471586702639,0.875255792173867),
 .UNSPECIFIED.);
#520=B_SPLINE_CURVE_WITH_KNOTS('',3,(#20783,#20784,#20785,#20786,#20787,
#20788,#20789,#20790,#20791,#20792),.UNSPECIFIED.,.F.,.F.,(4,2,2,2,4),(0.687371506923444,
0.701311490231616,0.76491921205255,0.828526933873483,0.842466917181656),
 .UNSPECIFIED.);
#521=B_SPLINE_CURVE_WITH_KNOTS('',3,(#20796,#20797,#20798,#20799,#20800,
#20801),.UNSPECIFIED.,.F.,.F.,(4,2,4),(0.254973070684183,0.318580792505117,
0.332520775813289),.UNSPECIFIED.);
#522=B_SPLINE_CURVE_WITH_KNOTS('',3,(#20805,#20806,#20807,#20808,#20809,
#20810,#20811,#20812,#20813,#20814,#20815,#20816,#20817,#20818,#20819,#20820,
#20821,#20822,#20823,#20824,#20825,#20826,#20827,#20828,#20829,#20830),
 .UNSPECIFIED.,.F.,.F.,(4,2,2,2,2,2,2,2,2,2,2,2,4),(0.,0.0622156192199746,
0.124431238439949,0.186646447577113,0.248861656714277,0.31107686585144,
0.373292074988604,0.435507694208578,0.497723313428553,0.559938932648528,
0.622154551868502,0.684369761005666,0.74658497014283),.UNSPECIFIED.);
#523=B_SPLINE_CURVE_WITH_KNOTS('',3,(#20831,#20832,#20833,#20834,#20835,
#20836,#20837,#20838,#20839,#20840),.UNSPECIFIED.,.F.,.F.,(4,2,2,2,4),(0.74658497014283,
0.808800179279993,0.871015388417157,0.933231007637132,0.995446626857106),
 .UNSPECIFIED.);
#524=B_SPLINE_CURVE_WITH_KNOTS('',3,(#20841,#20842,#20843,#20844,#20845,
#20846),.UNSPECIFIED.,.F.,.F.,(4,2,4),(0.177425365555079,0.19136534886325,
0.254973070684183),.UNSPECIFIED.);
#525=B_SPLINE_CURVE_WITH_KNOTS('',3,(#20892,#20893,#20894,#20895,#20896,
#20897,#20898,#20899,#20900,#20901),.UNSPECIFIED.,.F.,.F.,(4,2,2,2,4),(0.,
0.062275384959466,0.124550769918932,0.186824589898798,0.249098409878663),
 .UNSPECIFIED.);
#526=B_SPLINE_CURVE_WITH_KNOTS('',3,(#20902,#20903,#20904,#20905,#20906,
#20907,#20908,#20909,#20910,#20911,#20912,#20913,#20914,#20915,#20916,#20917,
#20918,#20919,#20920,#20921,#20922,#20923,#20924,#20925,#20926,#20927),
 .UNSPECIFIED.,.F.,.F.,(4,2,2,2,2,2,2,2,2,2,2,2,4),(0.249098409878663,0.311372229858529,
0.373646049838394,0.43592143479786,0.498196819757326,0.560472204716792,
0.622747589676259,0.685021409656124,0.74729522963599,0.809569049615855,
0.871842869595721,0.934118254555187,0.996393639514653),.UNSPECIFIED.);
#527=B_SPLINE_CURVE_WITH_KNOTS('',3,(#20931,#20932,#20933,#20934,#20935,
#20936,#20937,#20938,#20939,#20940,#20941,#20942,#20943,#20944,#20945,#20946,
#20947,#20948,#20949,#20950,#20951,#20952,#20953,#20954,#20955,#20956),
 .UNSPECIFIED.,.F.,.F.,(4,2,2,2,2,2,2,2,2,2,2,2,4),(0.,0.0621954302022363,
0.124390860404473,0.186586102839084,0.248781345273696,0.310976587708308,
0.37317183014292,0.435367260345156,0.497562690547392,0.559758120749629,
0.621953550951865,0.684148793386477,0.746344035821089),.UNSPECIFIED.);
#528=B_SPLINE_CURVE_WITH_KNOTS('',3,(#20957,#20958,#20959,#20960,#20961,
#20962,#20963,#20964,#20965,#20966),.UNSPECIFIED.,.F.,.F.,(4,2,2,2,4),(0.746344035821089,
0.8085392782557,0.870734520690312,0.932929950892549,0.995125381094785),
 .UNSPECIFIED.);
#529=SHAPE_REPRESENTATION_RELATIONSHIP('SRR','None',#33488,#574);
#530=SHAPE_REPRESENTATION_RELATIONSHIP('SRR','None',#33489,#575);
#531=SHAPE_REPRESENTATION_RELATIONSHIP('SRR','None',#33490,#576);
#532=SHAPE_REPRESENTATION_RELATIONSHIP('SRR','None',#33491,#577);
#533=SHAPE_REPRESENTATION_RELATIONSHIP('SRR','None',#33492,#578);
#534=SHAPE_REPRESENTATION_RELATIONSHIP('SRR','None',#33493,#579);
#535=SHAPE_REPRESENTATION_RELATIONSHIP('SRR','None',#33494,#580);
#536=SHAPE_REPRESENTATION_RELATIONSHIP('SRR','None',#33495,#581);
#537=SHAPE_REPRESENTATION_RELATIONSHIP('SRR','None',#33496,#582);
#538=SHAPE_REPRESENTATION_RELATIONSHIP('SRR','None',#33497,#583);
#539=SHAPE_REPRESENTATION_RELATIONSHIP('SRR','None',#33498,#584);
#540=SHAPE_REPRESENTATION_RELATIONSHIP('SRR','None',#33499,#585);
#541=SHAPE_REPRESENTATION_RELATIONSHIP('SRR','None',#33500,#586);
#542=SHAPE_REPRESENTATION_RELATIONSHIP('SRR','None',#33501,#587);
#543=SHAPE_REPRESENTATION_RELATIONSHIP('SRR','None',#33502,#588);
#544=SHAPE_REPRESENTATION_RELATIONSHIP('SRR','None',#33503,#589);
#545=SHAPE_REPRESENTATION_RELATIONSHIP('SRR','None',#33504,#590);
#546=SHAPE_REPRESENTATION_RELATIONSHIP('SRR','None',#33506,#591);
#547=SHAPE_REPRESENTATION_RELATIONSHIP('SRR','None',#33507,#592);
#548=SHAPE_REPRESENTATION_RELATIONSHIP('SRR','None',#33508,#593);
#549=SHAPE_REPRESENTATION_RELATIONSHIP('SRR','None',#33509,#594);
#550=SHAPE_REPRESENTATION_RELATIONSHIP('SRR','None',#33510,#595);
#551=SHAPE_REPRESENTATION_RELATIONSHIP('SRR','None',#33511,#596);
#552=SHAPE_REPRESENTATION_RELATIONSHIP('SRR','None',#33513,#597);
#553=SHAPE_REPRESENTATION_RELATIONSHIP('SRR','None',#33514,#598);
#554=SHAPE_REPRESENTATION_RELATIONSHIP('SRR','None',#33515,#599);
#555=SHAPE_REPRESENTATION_RELATIONSHIP('SRR','None',#33516,#600);
#556=SHAPE_REPRESENTATION_RELATIONSHIP('SRR','None',#33517,#601);
#557=SHAPE_REPRESENTATION_RELATIONSHIP('SRR','None',#33518,#602);
#558=SHAPE_REPRESENTATION_RELATIONSHIP('SRR','None',#33520,#603);
#559=SHAPE_REPRESENTATION_RELATIONSHIP('SRR','None',#33521,#604);
#560=SHAPE_REPRESENTATION_RELATIONSHIP('SRR','None',#33522,#605);
#561=SHAPE_REPRESENTATION_RELATIONSHIP('SRR','None',#33523,#606);
#562=SHAPE_REPRESENTATION_RELATIONSHIP('SRR','None',#33524,#607);
#563=SHAPE_REPRESENTATION_RELATIONSHIP('SRR','None',#33525,#608);
#564=SHAPE_REPRESENTATION_RELATIONSHIP('SRR','None',#33526,#609);
#565=SHAPE_REPRESENTATION_RELATIONSHIP('SRR','None',#33527,#610);
#566=SHAPE_REPRESENTATION_RELATIONSHIP('SRR','None',#33528,#611);
#567=SHAPE_REPRESENTATION_RELATIONSHIP('SRR','None',#33529,#612);
#568=SHAPE_REPRESENTATION_RELATIONSHIP('SRR','None',#33530,#613);
#569=SHAPE_REPRESENTATION_RELATIONSHIP('SRR','None',#33531,#614);
#570=SHAPE_REPRESENTATION_RELATIONSHIP('SRR','None',#33532,#615);
#571=SHAPE_REPRESENTATION_RELATIONSHIP('SRR','None',#33533,#616);
#572=SHAPE_REPRESENTATION_RELATIONSHIP('SRR','None',#33534,#617);
#573=SHAPE_REPRESENTATION_RELATIONSHIP('SRR','None',#33536,#618);
#574=ADVANCED_BREP_SHAPE_REPRESENTATION('',(#671),#33250);
#575=ADVANCED_BREP_SHAPE_REPRESENTATION('',(#672),#33251);
#576=ADVANCED_BREP_SHAPE_REPRESENTATION('',(#673),#33252);
#577=ADVANCED_BREP_SHAPE_REPRESENTATION('',(#674),#33253);
#578=ADVANCED_BREP_SHAPE_REPRESENTATION('',(#675),#33254);
#579=ADVANCED_BREP_SHAPE_REPRESENTATION('',(#676),#33255);
#580=ADVANCED_BREP_SHAPE_REPRESENTATION('',(#677),#33256);
#581=ADVANCED_BREP_SHAPE_REPRESENTATION('',(#678),#33257);
#582=ADVANCED_BREP_SHAPE_REPRESENTATION('',(#679),#33258);
#583=ADVANCED_BREP_SHAPE_REPRESENTATION('',(#680),#33259);
#584=ADVANCED_BREP_SHAPE_REPRESENTATION('',(#681),#33260);
#585=ADVANCED_BREP_SHAPE_REPRESENTATION('',(#682),#33261);
#586=ADVANCED_BREP_SHAPE_REPRESENTATION('',(#683),#33262);
#587=ADVANCED_BREP_SHAPE_REPRESENTATION('',(#684),#33263);
#588=ADVANCED_BREP_SHAPE_REPRESENTATION('',(#685),#33264);
#589=ADVANCED_BREP_SHAPE_REPRESENTATION('',(#686),#33265);
#590=ADVANCED_BREP_SHAPE_REPRESENTATION('',(#687),#33266);
#591=ADVANCED_BREP_SHAPE_REPRESENTATION('',(#688),#33268);
#592=ADVANCED_BREP_SHAPE_REPRESENTATION('',(#689),#33269);
#593=ADVANCED_BREP_SHAPE_REPRESENTATION('',(#690,#691,#692,#693,#694,#695,
#696),#33270);
#594=ADVANCED_BREP_SHAPE_REPRESENTATION('',(#697),#33271);
#595=ADVANCED_BREP_SHAPE_REPRESENTATION('',(#698,#699),#33272);
#596=ADVANCED_BREP_SHAPE_REPRESENTATION('',(#134),#33273);
#597=ADVANCED_BREP_SHAPE_REPRESENTATION('',(#700),#33275);
#598=ADVANCED_BREP_SHAPE_REPRESENTATION('',(#701),#33276);
#599=ADVANCED_BREP_SHAPE_REPRESENTATION('',(#702),#33277);
#600=ADVANCED_BREP_SHAPE_REPRESENTATION('',(#703),#33278);
#601=ADVANCED_BREP_SHAPE_REPRESENTATION('',(#704),#33279);
#602=ADVANCED_BREP_SHAPE_REPRESENTATION('',(#705),#33280);
#603=ADVANCED_BREP_SHAPE_REPRESENTATION('',(#706),#33282);
#604=ADVANCED_BREP_SHAPE_REPRESENTATION('',(#707),#33283);
#605=ADVANCED_BREP_SHAPE_REPRESENTATION('',(#708),#33284);
#606=ADVANCED_BREP_SHAPE_REPRESENTATION('',(#709),#33285);
#607=ADVANCED_BREP_SHAPE_REPRESENTATION('',(#710),#33286);
#608=ADVANCED_BREP_SHAPE_REPRESENTATION('',(#711),#33287);
#609=ADVANCED_BREP_SHAPE_REPRESENTATION('',(#712),#33288);
#610=ADVANCED_BREP_SHAPE_REPRESENTATION('',(#713),#33289);
#611=ADVANCED_BREP_SHAPE_REPRESENTATION('',(#714),#33290);
#612=ADVANCED_BREP_SHAPE_REPRESENTATION('',(#715),#33291);
#613=ADVANCED_BREP_SHAPE_REPRESENTATION('',(#716),#33292);
#614=ADVANCED_BREP_SHAPE_REPRESENTATION('',(#717),#33293);
#615=ADVANCED_BREP_SHAPE_REPRESENTATION('',(#718),#33294);
#616=ADVANCED_BREP_SHAPE_REPRESENTATION('',(#135),#33295);
#617=ADVANCED_BREP_SHAPE_REPRESENTATION('',(#136),#33296);
#618=ADVANCED_BREP_SHAPE_REPRESENTATION('',(#719),#33298);
#619=STYLED_ITEM('',(#33793),#671);
#620=STYLED_ITEM('',(#33800),#672);
#621=STYLED_ITEM('',(#33800),#673);
#622=STYLED_ITEM('',(#33793),#674);
#623=STYLED_ITEM('',(#33828),#675);
#624=STYLED_ITEM('',(#33807),#676);
#625=STYLED_ITEM('',(#33807),#677);
#626=STYLED_ITEM('',(#33807),#678);
#627=STYLED_ITEM('',(#33807),#679);
#628=STYLED_ITEM('',(#33807),#680);
#629=STYLED_ITEM('',(#33814),#681);
#630=STYLED_ITEM('',(#33814),#682);
#631=STYLED_ITEM('',(#33814),#683);
#632=STYLED_ITEM('',(#33814),#684);
#633=STYLED_ITEM('',(#33814),#685);
#634=STYLED_ITEM('',(#33814),#686);
#635=STYLED_ITEM('',(#33814),#687);
#636=STYLED_ITEM('',(#33814),#688);
#637=STYLED_ITEM('',(#33814),#689);
#638=STYLED_ITEM('',(#33814),#690);
#639=STYLED_ITEM('',(#33814),#691);
#640=STYLED_ITEM('',(#33814),#692);
#641=STYLED_ITEM('',(#33814),#693);
#642=STYLED_ITEM('',(#33814),#694);
#643=STYLED_ITEM('',(#33814),#695);
#644=STYLED_ITEM('',(#33814),#696);
#645=STYLED_ITEM('',(#33814),#697);
#646=STYLED_ITEM('',(#33814),#698);
#647=STYLED_ITEM('',(#33814),#699);
#648=STYLED_ITEM('',(#33821),#134);
#649=STYLED_ITEM('',(#33800),#700);
#650=STYLED_ITEM('',(#33807),#701);
#651=STYLED_ITEM('',(#33807),#702);
#652=STYLED_ITEM('',(#33821),#703);
#653=STYLED_ITEM('',(#33800),#704);
#654=STYLED_ITEM('',(#33821),#705);
#655=STYLED_ITEM('',(#33814),#706);
#656=STYLED_ITEM('',(#33814),#707);
#657=STYLED_ITEM('',(#33814),#708);
#658=STYLED_ITEM('',(#33814),#709);
#659=STYLED_ITEM('',(#33814),#710);
#660=STYLED_ITEM('',(#33814),#711);
#661=STYLED_ITEM('',(#33814),#712);
#662=STYLED_ITEM('',(#33800),#713);
#663=STYLED_ITEM('',(#33828),#714);
#664=STYLED_ITEM('',(#33814),#715);
#665=STYLED_ITEM('',(#33814),#716);
#666=STYLED_ITEM('',(#33828),#717);
#667=STYLED_ITEM('',(#33821),#718);
#668=STYLED_ITEM('',(#33821),#135);
#669=STYLED_ITEM('',(#33821),#136);
#670=STYLED_ITEM('',(#33821),#719);
#671=MANIFOLD_SOLID_BREP('Body1',#12637);
#672=MANIFOLD_SOLID_BREP('Body1',#12638);
#673=MANIFOLD_SOLID_BREP('Body1',#12639);
#674=MANIFOLD_SOLID_BREP('Body1',#12640);
#675=MANIFOLD_SOLID_BREP('Body1',#12641);
#676=MANIFOLD_SOLID_BREP('Body1',#12642);
#677=MANIFOLD_SOLID_BREP('Body1',#12643);
#678=MANIFOLD_SOLID_BREP('Body1',#12644);
#679=MANIFOLD_SOLID_BREP('Body1',#12645);
#680=MANIFOLD_SOLID_BREP('Body1',#12646);
#681=MANIFOLD_SOLID_BREP('Body1',#12647);
#682=MANIFOLD_SOLID_BREP('Body1',#12648);
#683=MANIFOLD_SOLID_BREP('Body1',#12649);
#684=MANIFOLD_SOLID_BREP('Body1',#12650);
#685=MANIFOLD_SOLID_BREP('Body1',#12651);
#686=MANIFOLD_SOLID_BREP('Body1',#12652);
#687=MANIFOLD_SOLID_BREP('Body1',#12653);
#688=MANIFOLD_SOLID_BREP('Body1',#12654);
#689=MANIFOLD_SOLID_BREP('Body1',#12655);
#690=MANIFOLD_SOLID_BREP('Body1',#12656);
#691=MANIFOLD_SOLID_BREP('Body2',#12657);
#692=MANIFOLD_SOLID_BREP('Body3',#12658);
#693=MANIFOLD_SOLID_BREP('Body4',#12659);
#694=MANIFOLD_SOLID_BREP('Body5',#12660);
#695=MANIFOLD_SOLID_BREP('Body6',#12661);
#696=MANIFOLD_SOLID_BREP('Body7',#12662);
#697=MANIFOLD_SOLID_BREP('Continuous crown cage',#12663);
#698=MANIFOLD_SOLID_BREP('Body1',#12664);
#699=MANIFOLD_SOLID_BREP('Body2',#12665);
#700=MANIFOLD_SOLID_BREP('Body1',#12668);
#701=MANIFOLD_SOLID_BREP('Body1',#12669);
#702=MANIFOLD_SOLID_BREP('Body1',#12670);
#703=MANIFOLD_SOLID_BREP('Body1',#12671);
#704=MANIFOLD_SOLID_BREP('Body1',#12672);
#705=MANIFOLD_SOLID_BREP('Body1',#12673);
#706=MANIFOLD_SOLID_BREP('Body1',#12674);
#707=MANIFOLD_SOLID_BREP('Body1',#12675);
#708=MANIFOLD_SOLID_BREP('Body1',#12676);
#709=MANIFOLD_SOLID_BREP('Body1',#12677);
#710=MANIFOLD_SOLID_BREP('Body1',#12678);
#711=MANIFOLD_SOLID_BREP('Body1',#12679);
#712=MANIFOLD_SOLID_BREP('Body1',#12680);
#713=MANIFOLD_SOLID_BREP('Body1',#12681);
#714=MANIFOLD_SOLID_BREP('Body1',#12682);
#715=MANIFOLD_SOLID_BREP('Body1',#12683);
#716=MANIFOLD_SOLID_BREP('Body1',#12684);
#717=MANIFOLD_SOLID_BREP('Body1',#12685);
#718=MANIFOLD_SOLID_BREP('Body1',#12686);
#719=MANIFOLD_SOLID_BREP('Body1',#12691);
#720=FACE_BOUND('',#2039,.T.);
#721=FACE_BOUND('',#2040,.T.);
#722=FACE_BOUND('',#2041,.T.);
#723=FACE_BOUND('',#2042,.T.);
#724=FACE_BOUND('',#2043,.T.);
#725=FACE_BOUND('',#2044,.T.);
#726=FACE_BOUND('',#2046,.T.);
#727=FACE_BOUND('',#2047,.T.);
#728=FACE_BOUND('',#2048,.T.);
#729=FACE_BOUND('',#2049,.T.);
#730=FACE_BOUND('',#2050,.T.);
#731=FACE_BOUND('',#2051,.T.);
#732=FACE_BOUND('',#2075,.T.);
#733=FACE_BOUND('',#2076,.T.);
#734=FACE_BOUND('',#2090,.T.);
#735=FACE_BOUND('',#2091,.T.);
#736=FACE_BOUND('',#2095,.T.);
#737=FACE_BOUND('',#2101,.T.);
#738=FACE_BOUND('',#2103,.T.);
#739=FACE_BOUND('',#2105,.T.);
#740=FACE_BOUND('',#2116,.T.);
#741=FACE_BOUND('',#2117,.T.);
#742=FACE_BOUND('',#2118,.T.);
#743=FACE_BOUND('',#2125,.T.);
#744=FACE_BOUND('',#2127,.T.);
#745=FACE_BOUND('',#2129,.T.);
#746=FACE_BOUND('',#2132,.T.);
#747=FACE_BOUND('',#2133,.T.);
#748=FACE_BOUND('',#2134,.T.);
#749=FACE_BOUND('',#2154,.T.);
#750=FACE_BOUND('',#2155,.T.);
#751=FACE_BOUND('',#2161,.T.);
#752=FACE_BOUND('',#2162,.T.);
#753=FACE_BOUND('',#2182,.T.);
#754=FACE_BOUND('',#2183,.T.);
#755=FACE_BOUND('',#2189,.T.);
#756=FACE_BOUND('',#2190,.T.);
#757=FACE_BOUND('',#2194,.T.);
#758=FACE_BOUND('',#2195,.T.);
#759=FACE_BOUND('',#2199,.T.);
#760=FACE_BOUND('',#2200,.T.);
#761=FACE_BOUND('',#2206,.T.);
#762=FACE_BOUND('',#2208,.T.);
#763=FACE_BOUND('',#2210,.T.);
#764=FACE_BOUND('',#2219,.T.);
#765=FACE_BOUND('',#2221,.T.);
#766=FACE_BOUND('',#2225,.T.);
#767=FACE_BOUND('',#2226,.T.);
#768=FACE_BOUND('',#2227,.T.);
#769=FACE_BOUND('',#2228,.T.);
#770=FACE_BOUND('',#2229,.T.);
#771=FACE_BOUND('',#2232,.T.);
#772=FACE_BOUND('',#2233,.T.);
#773=FACE_BOUND('',#2234,.T.);
#774=FACE_BOUND('',#2235,.T.);
#775=FACE_BOUND('',#2236,.T.);
#776=FACE_BOUND('',#2240,.T.);
#777=FACE_BOUND('',#2241,.T.);
#778=FACE_BOUND('',#2248,.T.);
#779=FACE_BOUND('',#2252,.T.);
#780=FACE_BOUND('',#2253,.T.);
#781=FACE_BOUND('',#2254,.T.);
#782=FACE_BOUND('',#2255,.T.);
#783=FACE_BOUND('',#2256,.T.);
#784=FACE_BOUND('',#2258,.T.);
#785=FACE_BOUND('',#2259,.T.);
#786=FACE_BOUND('',#2260,.T.);
#787=FACE_BOUND('',#2261,.T.);
#788=FACE_BOUND('',#2262,.T.);
#789=FACE_BOUND('',#2269,.T.);
#790=FACE_BOUND('',#2273,.T.);
#791=FACE_BOUND('',#2274,.T.);
#792=FACE_BOUND('',#2275,.T.);
#793=FACE_BOUND('',#2276,.T.);
#794=FACE_BOUND('',#2277,.T.);
#795=FACE_BOUND('',#2279,.T.);
#796=FACE_BOUND('',#2280,.T.);
#797=FACE_BOUND('',#2281,.T.);
#798=FACE_BOUND('',#2282,.T.);
#799=FACE_BOUND('',#2283,.T.);
#800=FACE_BOUND('',#2292,.T.);
#801=FACE_BOUND('',#2294,.T.);
#802=FACE_BOUND('',#2298,.T.);
#803=FACE_BOUND('',#2299,.T.);
#804=FACE_BOUND('',#2300,.T.);
#805=FACE_BOUND('',#2301,.T.);
#806=FACE_BOUND('',#2302,.T.);
#807=FACE_BOUND('',#2305,.T.);
#808=FACE_BOUND('',#2306,.T.);
#809=FACE_BOUND('',#2307,.T.);
#810=FACE_BOUND('',#2308,.T.);
#811=FACE_BOUND('',#2309,.T.);
#812=FACE_BOUND('',#2313,.T.);
#813=FACE_BOUND('',#2314,.T.);
#814=FACE_BOUND('',#2321,.T.);
#815=FACE_BOUND('',#2325,.T.);
#816=FACE_BOUND('',#2326,.T.);
#817=FACE_BOUND('',#2327,.T.);
#818=FACE_BOUND('',#2328,.T.);
#819=FACE_BOUND('',#2329,.T.);
#820=FACE_BOUND('',#2331,.T.);
#821=FACE_BOUND('',#2332,.T.);
#822=FACE_BOUND('',#2333,.T.);
#823=FACE_BOUND('',#2334,.T.);
#824=FACE_BOUND('',#2335,.T.);
#825=FACE_BOUND('',#2342,.T.);
#826=FACE_BOUND('',#2346,.T.);
#827=FACE_BOUND('',#2347,.T.);
#828=FACE_BOUND('',#2348,.T.);
#829=FACE_BOUND('',#2349,.T.);
#830=FACE_BOUND('',#2350,.T.);
#831=FACE_BOUND('',#2352,.T.);
#832=FACE_BOUND('',#2353,.T.);
#833=FACE_BOUND('',#2354,.T.);
#834=FACE_BOUND('',#2355,.T.);
#835=FACE_BOUND('',#2356,.T.);
#836=FACE_BOUND('',#2366,.T.);
#837=FACE_BOUND('',#2369,.T.);
#838=FACE_BOUND('',#2374,.T.);
#839=FACE_BOUND('',#2379,.T.);
#840=FACE_BOUND('',#2404,.T.);
#841=FACE_BOUND('',#2407,.T.);
#842=FACE_BOUND('',#2410,.T.);
#843=FACE_BOUND('',#2413,.T.);
#844=FACE_BOUND('',#2416,.T.);
#845=FACE_BOUND('',#2432,.T.);
#846=FACE_BOUND('',#2607,.T.);
#847=FACE_BOUND('',#2612,.T.);
#848=FACE_BOUND('',#2615,.T.);
#849=FACE_BOUND('',#2617,.T.);
#850=FACE_BOUND('',#2619,.T.);
#851=FACE_BOUND('',#2621,.T.);
#852=FACE_BOUND('',#2635,.T.);
#853=FACE_BOUND('',#2637,.T.);
#854=FACE_BOUND('',#2647,.T.);
#855=FACE_BOUND('',#2667,.T.);
#856=FACE_BOUND('',#2668,.T.);
#857=FACE_BOUND('',#2670,.T.);
#858=FACE_BOUND('',#2672,.T.);
#859=FACE_BOUND('',#2676,.T.);
#860=FACE_BOUND('',#2678,.T.);
#861=FACE_BOUND('',#2682,.T.);
#862=FACE_BOUND('',#2684,.T.);
#863=FACE_BOUND('',#2688,.T.);
#864=FACE_BOUND('',#2690,.T.);
#865=FACE_BOUND('',#2694,.T.);
#866=FACE_BOUND('',#2696,.T.);
#867=FACE_BOUND('',#2714,.T.);
#868=FACE_BOUND('',#2719,.T.);
#869=FACE_BOUND('',#2722,.T.);
#870=FACE_BOUND('',#2724,.T.);
#871=FACE_BOUND('',#2726,.T.);
#872=FACE_BOUND('',#2730,.T.);
#873=FACE_BOUND('',#2732,.T.);
#874=FACE_BOUND('',#2736,.T.);
#875=FACE_BOUND('',#2738,.T.);
#876=FACE_BOUND('',#2742,.T.);
#877=FACE_BOUND('',#2744,.T.);
#878=FACE_BOUND('',#2749,.T.);
#879=FACE_BOUND('',#2753,.T.);
#880=FACE_BOUND('',#2834,.T.);
#881=FACE_BOUND('',#2839,.T.);
#882=FACE_BOUND('',#2841,.T.);
#883=FACE_BOUND('',#2847,.T.);
#884=FACE_BOUND('',#2865,.T.);
#885=FACE_BOUND('',#2881,.T.);
#886=FACE_BOUND('',#2883,.T.);
#887=PLANE('',#13209);
#888=PLANE('',#13210);
#889=PLANE('',#13211);
#890=PLANE('',#13212);
#891=PLANE('',#13213);
#892=PLANE('',#13214);
#893=PLANE('',#13216);
#894=PLANE('',#13217);
#895=PLANE('',#13218);
#896=PLANE('',#13219);
#897=PLANE('',#13220);
#898=PLANE('',#13221);
#899=PLANE('',#13223);
#900=PLANE('',#13224);
#901=PLANE('',#13225);
#902=PLANE('',#13226);
#903=PLANE('',#13227);
#904=PLANE('',#13228);
#905=PLANE('',#13233);
#906=PLANE('',#13237);
#907=PLANE('',#13238);
#908=PLANE('',#13239);
#909=PLANE('',#13240);
#910=PLANE('',#13250);
#911=PLANE('',#13251);
#912=PLANE('',#13252);
#913=PLANE('',#13256);
#914=PLANE('',#13260);
#915=PLANE('',#13261);
#916=PLANE('',#13262);
#917=PLANE('',#13263);
#918=PLANE('',#13275);
#919=PLANE('',#13276);
#920=PLANE('',#13277);
#921=PLANE('',#13278);
#922=PLANE('',#13279);
#923=PLANE('',#13283);
#924=PLANE('',#13284);
#925=PLANE('',#13291);
#926=PLANE('',#13292);
#927=PLANE('',#13293);
#928=PLANE('',#13294);
#929=PLANE('',#13295);
#930=PLANE('',#13296);
#931=PLANE('',#13301);
#932=PLANE('',#13306);
#933=PLANE('',#13308);
#934=PLANE('',#13315);
#935=PLANE('',#13319);
#936=PLANE('',#13326);
#937=PLANE('',#13332);
#938=PLANE('',#13334);
#939=PLANE('',#13335);
#940=PLANE('',#13336);
#941=PLANE('',#13337);
#942=PLANE('',#13338);
#943=PLANE('',#13345);
#944=PLANE('',#13349);
#945=PLANE('',#13357);
#946=PLANE('',#13358);
#947=PLANE('',#13359);
#948=PLANE('',#13360);
#949=PLANE('',#13361);
#950=PLANE('',#13362);
#951=PLANE('',#13363);
#952=PLANE('',#13367);
#953=PLANE('',#13368);
#954=PLANE('',#13369);
#955=PLANE('',#13370);
#956=PLANE('',#13372);
#957=PLANE('',#13373);
#958=PLANE('',#13374);
#959=PLANE('',#13375);
#960=PLANE('',#13376);
#961=PLANE('',#13383);
#962=PLANE('',#13387);
#963=PLANE('',#13395);
#964=PLANE('',#13396);
#965=PLANE('',#13397);
#966=PLANE('',#13398);
#967=PLANE('',#13399);
#968=PLANE('',#13400);
#969=PLANE('',#13401);
#970=PLANE('',#13405);
#971=PLANE('',#13406);
#972=PLANE('',#13407);
#973=PLANE('',#13408);
#974=PLANE('',#13410);
#975=PLANE('',#13411);
#976=PLANE('',#13412);
#977=PLANE('',#13415);
#978=PLANE('',#13416);
#979=PLANE('',#13417);
#980=PLANE('',#13420);
#981=PLANE('',#13424);
#982=PLANE('',#13430);
#983=PLANE('',#13453);
#984=PLANE('',#13454);
#985=PLANE('',#13455);
#986=PLANE('',#13456);
#987=PLANE('',#13457);
#988=PLANE('',#13458);
#989=PLANE('',#13459);
#990=PLANE('',#13460);
#991=PLANE('',#13461);
#992=PLANE('',#13462);
#993=PLANE('',#13479);
#994=PLANE('',#13486);
#995=PLANE('',#13487);
#996=PLANE('',#13504);
#997=PLANE('',#13511);
#998=PLANE('',#13512);
#999=PLANE('',#13535);
#1000=PLANE('',#13536);
#1001=PLANE('',#13537);
#1002=PLANE('',#13538);
#1003=PLANE('',#13539);
#1004=PLANE('',#13540);
#1005=PLANE('',#13541);
#1006=PLANE('',#13542);
#1007=PLANE('',#13543);
#1008=PLANE('',#13544);
#1009=PLANE('',#13561);
#1010=PLANE('',#13568);
#1011=PLANE('',#13569);
#1012=PLANE('',#13586);
#1013=PLANE('',#13593);
#1014=PLANE('',#13594);
#1015=PLANE('',#13596);
#1016=PLANE('',#13602);
#1017=PLANE('',#13618);
#1018=PLANE('',#13621);
#1019=PLANE('',#13633);
#1020=PLANE('',#13642);
#1021=PLANE('',#13673);
#1022=PLANE('',#13678);
#1023=PLANE('',#13683);
#1024=PLANE('',#13689);
#1025=PLANE('',#13694);
#1026=PLANE('',#13703);
#1027=PLANE('',#13707);
#1028=PLANE('',#13708);
#1029=PLANE('',#13710);
#1030=PLANE('',#13715);
#1031=PLANE('',#13718);
#1032=PLANE('',#13723);
#1033=PLANE('',#13732);
#1034=PLANE('',#13733);
#1035=PLANE('',#13734);
#1036=PLANE('',#13735);
#1037=PLANE('',#13736);
#1038=PLANE('',#13737);
#1039=PLANE('',#13738);
#1040=PLANE('',#13739);
#1041=PLANE('',#13740);
#1042=PLANE('',#13742);
#1043=PLANE('',#13750);
#1044=PLANE('',#13760);
#1045=PLANE('',#13761);
#1046=PLANE('',#13762);
#1047=PLANE('',#13763);
#1048=PLANE('',#13766);
#1049=PLANE('',#13769);
#1050=PLANE('',#13770);
#1051=PLANE('',#13771);
#1052=PLANE('',#13772);
#1053=PLANE('',#13773);
#1054=PLANE('',#13774);
#1055=PLANE('',#13775);
#1056=PLANE('',#13776);
#1057=PLANE('',#13777);
#1058=PLANE('',#13778);
#1059=PLANE('',#13779);
#1060=PLANE('',#13780);
#1061=PLANE('',#13781);
#1062=PLANE('',#13782);
#1063=PLANE('',#13783);
#1064=PLANE('',#13784);
#1065=PLANE('',#13785);
#1066=PLANE('',#13786);
#1067=PLANE('',#13787);
#1068=PLANE('',#13788);
#1069=PLANE('',#13789);
#1070=PLANE('',#13790);
#1071=PLANE('',#13791);
#1072=PLANE('',#13792);
#1073=PLANE('',#13793);
#1074=PLANE('',#13794);
#1075=PLANE('',#13795);
#1076=PLANE('',#13796);
#1077=PLANE('',#13797);
#1078=PLANE('',#13798);
#1079=PLANE('',#13799);
#1080=PLANE('',#13800);
#1081=PLANE('',#13801);
#1082=PLANE('',#13802);
#1083=PLANE('',#13803);
#1084=PLANE('',#13804);
#1085=PLANE('',#13805);
#1086=PLANE('',#13806);
#1087=PLANE('',#13807);
#1088=PLANE('',#13808);
#1089=PLANE('',#13809);
#1090=PLANE('',#13810);
#1091=PLANE('',#13811);
#1092=PLANE('',#13812);
#1093=PLANE('',#13813);
#1094=PLANE('',#13814);
#1095=PLANE('',#13815);
#1096=PLANE('',#13816);
#1097=PLANE('',#13817);
#1098=PLANE('',#13818);
#1099=PLANE('',#13819);
#1100=PLANE('',#13820);
#1101=PLANE('',#13821);
#1102=PLANE('',#13822);
#1103=PLANE('',#13823);
#1104=PLANE('',#13824);
#1105=PLANE('',#13825);
#1106=PLANE('',#13826);
#1107=PLANE('',#13827);
#1108=PLANE('',#13828);
#1109=PLANE('',#13829);
#1110=PLANE('',#13830);
#1111=PLANE('',#13831);
#1112=PLANE('',#13832);
#1113=PLANE('',#13833);
#1114=PLANE('',#13834);
#1115=PLANE('',#13835);
#1116=PLANE('',#13836);
#1117=PLANE('',#13837);
#1118=PLANE('',#13838);
#1119=PLANE('',#13839);
#1120=PLANE('',#13840);
#1121=PLANE('',#13841);
#1122=PLANE('',#13842);
#1123=PLANE('',#13843);
#1124=PLANE('',#13844);
#1125=PLANE('',#13845);
#1126=PLANE('',#13846);
#1127=PLANE('',#13847);
#1128=PLANE('',#13848);
#1129=PLANE('',#13849);
#1130=PLANE('',#13850);
#1131=PLANE('',#13851);
#1132=PLANE('',#13852);
#1133=PLANE('',#13853);
#1134=PLANE('',#13854);
#1135=PLANE('',#13855);
#1136=PLANE('',#13856);
#1137=PLANE('',#13857);
#1138=PLANE('',#13858);
#1139=PLANE('',#13859);
#1140=PLANE('',#13860);
#1141=PLANE('',#13861);
#1142=PLANE('',#13862);
#1143=PLANE('',#13863);
#1144=PLANE('',#13864);
#1145=PLANE('',#13865);
#1146=PLANE('',#13866);
#1147=PLANE('',#13867);
#1148=PLANE('',#13868);
#1149=PLANE('',#13869);
#1150=PLANE('',#13870);
#1151=PLANE('',#13871);
#1152=PLANE('',#13872);
#1153=PLANE('',#13873);
#1154=PLANE('',#13874);
#1155=PLANE('',#13875);
#1156=PLANE('',#13876);
#1157=PLANE('',#13877);
#1158=PLANE('',#13878);
#1159=PLANE('',#13879);
#1160=PLANE('',#13880);
#1161=PLANE('',#13881);
#1162=PLANE('',#13882);
#1163=PLANE('',#13883);
#1164=PLANE('',#13884);
#1165=PLANE('',#13885);
#1166=PLANE('',#13886);
#1167=PLANE('',#13887);
#1168=PLANE('',#13888);
#1169=PLANE('',#13889);
#1170=PLANE('',#13890);
#1171=PLANE('',#13891);
#1172=PLANE('',#13892);
#1173=PLANE('',#13893);
#1174=PLANE('',#13894);
#1175=PLANE('',#13895);
#1176=PLANE('',#13896);
#1177=PLANE('',#13897);
#1178=PLANE('',#13898);
#1179=PLANE('',#13899);
#1180=PLANE('',#13900);
#1181=PLANE('',#13901);
#1182=PLANE('',#13902);
#1183=PLANE('',#13903);
#1184=PLANE('',#13904);
#1185=PLANE('',#13905);
#1186=PLANE('',#13906);
#1187=PLANE('',#13907);
#1188=PLANE('',#13908);
#1189=PLANE('',#13909);
#1190=PLANE('',#13910);
#1191=PLANE('',#13911);
#1192=PLANE('',#13912);
#1193=PLANE('',#13913);
#1194=PLANE('',#13914);
#1195=PLANE('',#13915);
#1196=PLANE('',#13916);
#1197=PLANE('',#13917);
#1198=PLANE('',#13918);
#1199=PLANE('',#13919);
#1200=PLANE('',#13920);
#1201=PLANE('',#13921);
#1202=PLANE('',#13922);
#1203=PLANE('',#13923);
#1204=PLANE('',#13924);
#1205=PLANE('',#13925);
#1206=PLANE('',#13926);
#1207=PLANE('',#13927);
#1208=PLANE('',#13928);
#1209=PLANE('',#13929);
#1210=PLANE('',#13930);
#1211=PLANE('',#13931);
#1212=PLANE('',#13935);
#1213=PLANE('',#13936);
#1214=PLANE('',#13938);
#1215=PLANE('',#13942);
#1216=PLANE('',#13949);
#1217=PLANE('',#13953);
#1218=PLANE('',#13954);
#1219=PLANE('',#13959);
#1220=PLANE('',#13960);
#1221=PLANE('',#13965);
#1222=PLANE('',#13966);
#1223=PLANE('',#13969);
#1224=PLANE('',#13970);
#1225=PLANE('',#13971);
#1226=PLANE('',#13972);
#1227=PLANE('',#13973);
#1228=PLANE('',#13980);
#1229=PLANE('',#13982);
#1230=PLANE('',#13983);
#1231=PLANE('',#13984);
#1232=PLANE('',#13985);
#1233=PLANE('',#13986);
#1234=PLANE('',#13987);
#1235=PLANE('',#13988);
#1236=PLANE('',#13989);
#1237=PLANE('',#13997);
#1238=PLANE('',#14009);
#1239=PLANE('',#14013);
#1240=PLANE('',#14014);
#1241=PLANE('',#14015);
#1242=PLANE('',#14017);
#1243=PLANE('',#14018);
#1244=PLANE('',#14019);
#1245=PLANE('',#14021);
#1246=PLANE('',#14022);
#1247=PLANE('',#14024);
#1248=PLANE('',#14025);
#1249=PLANE('',#14026);
#1250=PLANE('',#14031);
#1251=PLANE('',#14032);
#1252=PLANE('',#14040);
#1253=PLANE('',#14041);
#1254=PLANE('',#14049);
#1255=PLANE('',#14050);
#1256=PLANE('',#14058);
#1257=PLANE('',#14059);
#1258=PLANE('',#14067);
#1259=PLANE('',#14068);
#1260=PLANE('',#14070);
#1261=PLANE('',#14071);
#1262=PLANE('',#14072);
#1263=PLANE('',#14073);
#1264=PLANE('',#14074);
#1265=PLANE('',#14075);
#1266=PLANE('',#14077);
#1267=PLANE('',#14078);
#1268=PLANE('',#14079);
#1269=PLANE('',#14080);
#1270=PLANE('',#14081);
#1271=PLANE('',#14082);
#1272=PLANE('',#14087);
#1273=PLANE('',#14088);
#1274=PLANE('',#14089);
#1275=PLANE('',#14090);
#1276=PLANE('',#14098);
#1277=PLANE('',#14099);
#1278=PLANE('',#14101);
#1279=PLANE('',#14102);
#1280=PLANE('',#14106);
#1281=PLANE('',#14114);
#1282=PLANE('',#14115);
#1283=PLANE('',#14123);
#1284=PLANE('',#14124);
#1285=PLANE('',#14132);
#1286=PLANE('',#14133);
#1287=PLANE('',#14135);
#1288=PLANE('',#14136);
#1289=PLANE('',#14137);
#1290=PLANE('',#14138);
#1291=PLANE('',#14165);
#1292=PLANE('',#14166);
#1293=PLANE('',#14169);
#1294=PLANE('',#14172);
#1295=PLANE('',#14175);
#1296=PLANE('',#14178);
#1297=PLANE('',#14181);
#1298=PLANE('',#14184);
#1299=PLANE('',#14187);
#1300=PLANE('',#14190);
#1301=PLANE('',#14193);
#1302=PLANE('',#14196);
#1303=PLANE('',#14199);
#1304=PLANE('',#14202);
#1305=PLANE('',#14205);
#1306=PLANE('',#14208);
#1307=PLANE('',#14211);
#1308=PLANE('',#14214);
#1309=PLANE('',#14217);
#1310=PLANE('',#14220);
#1311=PLANE('',#14223);
#1312=PLANE('',#14224);
#1313=PLANE('',#14234);
#1314=PLANE('',#14235);
#1315=PLANE('',#14237);
#1316=PLANE('',#14245);
#1317=PLANE('',#14253);
#1318=PLANE('',#14254);
#1319=PLANE('',#14255);
#1320=PLANE('',#14256);
#1321=PLANE('',#14257);
#1322=PLANE('',#14258);
#1323=PLANE('',#14259);
#1324=PLANE('',#14260);
#1325=PLANE('',#14261);
#1326=PLANE('',#14263);
#1327=PLANE('',#14271);
#1328=PLANE('',#14279);
#1329=PLANE('',#14280);
#1330=PLANE('',#14281);
#1331=PLANE('',#14282);
#1332=PLANE('',#14283);
#1333=PLANE('',#14284);
#1334=PLANE('',#14285);
#1335=PLANE('',#14286);
#1336=PLANE('',#14287);
#1337=PLANE('',#14360);
#1338=PLANE('',#14361);
#1339=FACE_OUTER_BOUND('',#2028,.T.);
#1340=FACE_OUTER_BOUND('',#2029,.T.);
#1341=FACE_OUTER_BOUND('',#2030,.T.);
#1342=FACE_OUTER_BOUND('',#2031,.T.);
#1343=FACE_OUTER_BOUND('',#2032,.T.);
#1344=FACE_OUTER_BOUND('',#2033,.T.);
#1345=FACE_OUTER_BOUND('',#2034,.T.);
#1346=FACE_OUTER_BOUND('',#2035,.T.);
#1347=FACE_OUTER_BOUND('',#2036,.T.);
#1348=FACE_OUTER_BOUND('',#2037,.T.);
#1349=FACE_OUTER_BOUND('',#2038,.T.);
#1350=FACE_OUTER_BOUND('',#2045,.T.);
#1351=FACE_OUTER_BOUND('',#2052,.T.);
#1352=FACE_OUTER_BOUND('',#2053,.T.);
#1353=FACE_OUTER_BOUND('',#2054,.T.);
#1354=FACE_OUTER_BOUND('',#2055,.T.);
#1355=FACE_OUTER_BOUND('',#2056,.T.);
#1356=FACE_OUTER_BOUND('',#2057,.T.);
#1357=FACE_OUTER_BOUND('',#2058,.T.);
#1358=FACE_OUTER_BOUND('',#2059,.T.);
#1359=FACE_OUTER_BOUND('',#2060,.T.);
#1360=FACE_OUTER_BOUND('',#2061,.T.);
#1361=FACE_OUTER_BOUND('',#2062,.T.);
#1362=FACE_OUTER_BOUND('',#2063,.T.);
#1363=FACE_OUTER_BOUND('',#2064,.T.);
#1364=FACE_OUTER_BOUND('',#2065,.T.);
#1365=FACE_OUTER_BOUND('',#2066,.T.);
#1366=FACE_OUTER_BOUND('',#2067,.T.);
#1367=FACE_OUTER_BOUND('',#2068,.T.);
#1368=FACE_OUTER_BOUND('',#2069,.T.);
#1369=FACE_OUTER_BOUND('',#2070,.T.);
#1370=FACE_OUTER_BOUND('',#2071,.T.);
#1371=FACE_OUTER_BOUND('',#2072,.T.);
#1372=FACE_OUTER_BOUND('',#2073,.T.);
#1373=FACE_OUTER_BOUND('',#2074,.T.);
#1374=FACE_OUTER_BOUND('',#2077,.T.);
#1375=FACE_OUTER_BOUND('',#2078,.T.);
#1376=FACE_OUTER_BOUND('',#2079,.T.);
#1377=FACE_OUTER_BOUND('',#2080,.T.);
#1378=FACE_OUTER_BOUND('',#2081,.T.);
#1379=FACE_OUTER_BOUND('',#2082,.T.);
#1380=FACE_OUTER_BOUND('',#2083,.T.);
#1381=FACE_OUTER_BOUND('',#2084,.T.);
#1382=FACE_OUTER_BOUND('',#2085,.T.);
#1383=FACE_OUTER_BOUND('',#2086,.T.);
#1384=FACE_OUTER_BOUND('',#2087,.T.);
#1385=FACE_OUTER_BOUND('',#2088,.T.);
#1386=FACE_OUTER_BOUND('',#2089,.T.);
#1387=FACE_OUTER_BOUND('',#2092,.T.);
#1388=FACE_OUTER_BOUND('',#2093,.T.);
#1389=FACE_OUTER_BOUND('',#2094,.T.);
#1390=FACE_OUTER_BOUND('',#2096,.T.);
#1391=FACE_OUTER_BOUND('',#2097,.T.);
#1392=FACE_OUTER_BOUND('',#2098,.T.);
#1393=FACE_OUTER_BOUND('',#2099,.T.);
#1394=FACE_OUTER_BOUND('',#2100,.T.);
#1395=FACE_OUTER_BOUND('',#2102,.T.);
#1396=FACE_OUTER_BOUND('',#2104,.T.);
#1397=FACE_OUTER_BOUND('',#2106,.T.);
#1398=FACE_OUTER_BOUND('',#2107,.T.);
#1399=FACE_OUTER_BOUND('',#2108,.T.);
#1400=FACE_OUTER_BOUND('',#2109,.T.);
#1401=FACE_OUTER_BOUND('',#2110,.T.);
#1402=FACE_OUTER_BOUND('',#2111,.T.);
#1403=FACE_OUTER_BOUND('',#2112,.T.);
#1404=FACE_OUTER_BOUND('',#2113,.T.);
#1405=FACE_OUTER_BOUND('',#2114,.T.);
#1406=FACE_OUTER_BOUND('',#2115,.T.);
#1407=FACE_OUTER_BOUND('',#2119,.T.);
#1408=FACE_OUTER_BOUND('',#2120,.T.);
#1409=FACE_OUTER_BOUND('',#2121,.T.);
#1410=FACE_OUTER_BOUND('',#2122,.T.);
#1411=FACE_OUTER_BOUND('',#2123,.T.);
#1412=FACE_OUTER_BOUND('',#2124,.T.);
#1413=FACE_OUTER_BOUND('',#2126,.T.);
#1414=FACE_OUTER_BOUND('',#2128,.T.);
#1415=FACE_OUTER_BOUND('',#2130,.T.);
#1416=FACE_OUTER_BOUND('',#2131,.T.);
#1417=FACE_OUTER_BOUND('',#2135,.T.);
#1418=FACE_OUTER_BOUND('',#2136,.T.);
#1419=FACE_OUTER_BOUND('',#2137,.T.);
#1420=FACE_OUTER_BOUND('',#2138,.T.);
#1421=FACE_OUTER_BOUND('',#2139,.T.);
#1422=FACE_OUTER_BOUND('',#2140,.T.);
#1423=FACE_OUTER_BOUND('',#2141,.T.);
#1424=FACE_OUTER_BOUND('',#2142,.T.);
#1425=FACE_OUTER_BOUND('',#2143,.T.);
#1426=FACE_OUTER_BOUND('',#2144,.T.);
#1427=FACE_OUTER_BOUND('',#2145,.T.);
#1428=FACE_OUTER_BOUND('',#2146,.T.);
#1429=FACE_OUTER_BOUND('',#2147,.T.);
#1430=FACE_OUTER_BOUND('',#2148,.T.);
#1431=FACE_OUTER_BOUND('',#2149,.T.);
#1432=FACE_OUTER_BOUND('',#2150,.T.);
#1433=FACE_OUTER_BOUND('',#2151,.T.);
#1434=FACE_OUTER_BOUND('',#2152,.T.);
#1435=FACE_OUTER_BOUND('',#2153,.T.);
#1436=FACE_OUTER_BOUND('',#2156,.T.);
#1437=FACE_OUTER_BOUND('',#2157,.T.);
#1438=FACE_OUTER_BOUND('',#2158,.T.);
#1439=FACE_OUTER_BOUND('',#2159,.T.);
#1440=FACE_OUTER_BOUND('',#2160,.T.);
#1441=FACE_OUTER_BOUND('',#2163,.T.);
#1442=FACE_OUTER_BOUND('',#2164,.T.);
#1443=FACE_OUTER_BOUND('',#2165,.T.);
#1444=FACE_OUTER_BOUND('',#2166,.T.);
#1445=FACE_OUTER_BOUND('',#2167,.T.);
#1446=FACE_OUTER_BOUND('',#2168,.T.);
#1447=FACE_OUTER_BOUND('',#2169,.T.);
#1448=FACE_OUTER_BOUND('',#2170,.T.);
#1449=FACE_OUTER_BOUND('',#2171,.T.);
#1450=FACE_OUTER_BOUND('',#2172,.T.);
#1451=FACE_OUTER_BOUND('',#2173,.T.);
#1452=FACE_OUTER_BOUND('',#2174,.T.);
#1453=FACE_OUTER_BOUND('',#2175,.T.);
#1454=FACE_OUTER_BOUND('',#2176,.T.);
#1455=FACE_OUTER_BOUND('',#2177,.T.);
#1456=FACE_OUTER_BOUND('',#2178,.T.);
#1457=FACE_OUTER_BOUND('',#2179,.T.);
#1458=FACE_OUTER_BOUND('',#2180,.T.);
#1459=FACE_OUTER_BOUND('',#2181,.T.);
#1460=FACE_OUTER_BOUND('',#2184,.T.);
#1461=FACE_OUTER_BOUND('',#2185,.T.);
#1462=FACE_OUTER_BOUND('',#2186,.T.);
#1463=FACE_OUTER_BOUND('',#2187,.T.);
#1464=FACE_OUTER_BOUND('',#2188,.T.);
#1465=FACE_OUTER_BOUND('',#2191,.T.);
#1466=FACE_OUTER_BOUND('',#2192,.T.);
#1467=FACE_OUTER_BOUND('',#2193,.T.);
#1468=FACE_OUTER_BOUND('',#2196,.T.);
#1469=FACE_OUTER_BOUND('',#2197,.T.);
#1470=FACE_OUTER_BOUND('',#2198,.T.);
#1471=FACE_OUTER_BOUND('',#2201,.T.);
#1472=FACE_OUTER_BOUND('',#2202,.T.);
#1473=FACE_OUTER_BOUND('',#2203,.T.);
#1474=FACE_OUTER_BOUND('',#2204,.T.);
#1475=FACE_OUTER_BOUND('',#2205,.T.);
#1476=FACE_OUTER_BOUND('',#2207,.T.);
#1477=FACE_OUTER_BOUND('',#2209,.T.);
#1478=FACE_OUTER_BOUND('',#2211,.T.);
#1479=FACE_OUTER_BOUND('',#2212,.T.);
#1480=FACE_OUTER_BOUND('',#2213,.T.);
#1481=FACE_OUTER_BOUND('',#2214,.T.);
#1482=FACE_OUTER_BOUND('',#2215,.T.);
#1483=FACE_OUTER_BOUND('',#2216,.T.);
#1484=FACE_OUTER_BOUND('',#2217,.T.);
#1485=FACE_OUTER_BOUND('',#2218,.T.);
#1486=FACE_OUTER_BOUND('',#2220,.T.);
#1487=FACE_OUTER_BOUND('',#2222,.T.);
#1488=FACE_OUTER_BOUND('',#2223,.T.);
#1489=FACE_OUTER_BOUND('',#2224,.T.);
#1490=FACE_OUTER_BOUND('',#2230,.T.);
#1491=FACE_OUTER_BOUND('',#2231,.T.);
#1492=FACE_OUTER_BOUND('',#2237,.T.);
#1493=FACE_OUTER_BOUND('',#2238,.T.);
#1494=FACE_OUTER_BOUND('',#2239,.T.);
#1495=FACE_OUTER_BOUND('',#2242,.T.);
#1496=FACE_OUTER_BOUND('',#2243,.T.);
#1497=FACE_OUTER_BOUND('',#2244,.T.);
#1498=FACE_OUTER_BOUND('',#2245,.T.);
#1499=FACE_OUTER_BOUND('',#2246,.T.);
#1500=FACE_OUTER_BOUND('',#2247,.T.);
#1501=FACE_OUTER_BOUND('',#2249,.T.);
#1502=FACE_OUTER_BOUND('',#2250,.T.);
#1503=FACE_OUTER_BOUND('',#2251,.T.);
#1504=FACE_OUTER_BOUND('',#2257,.T.);
#1505=FACE_OUTER_BOUND('',#2263,.T.);
#1506=FACE_OUTER_BOUND('',#2264,.T.);
#1507=FACE_OUTER_BOUND('',#2265,.T.);
#1508=FACE_OUTER_BOUND('',#2266,.T.);
#1509=FACE_OUTER_BOUND('',#2267,.T.);
#1510=FACE_OUTER_BOUND('',#2268,.T.);
#1511=FACE_OUTER_BOUND('',#2270,.T.);
#1512=FACE_OUTER_BOUND('',#2271,.T.);
#1513=FACE_OUTER_BOUND('',#2272,.T.);
#1514=FACE_OUTER_BOUND('',#2278,.T.);
#1515=FACE_OUTER_BOUND('',#2284,.T.);
#1516=FACE_OUTER_BOUND('',#2285,.T.);
#1517=FACE_OUTER_BOUND('',#2286,.T.);
#1518=FACE_OUTER_BOUND('',#2287,.T.);
#1519=FACE_OUTER_BOUND('',#2288,.T.);
#1520=FACE_OUTER_BOUND('',#2289,.T.);
#1521=FACE_OUTER_BOUND('',#2290,.T.);
#1522=FACE_OUTER_BOUND('',#2291,.T.);
#1523=FACE_OUTER_BOUND('',#2293,.T.);
#1524=FACE_OUTER_BOUND('',#2295,.T.);
#1525=FACE_OUTER_BOUND('',#2296,.T.);
#1526=FACE_OUTER_BOUND('',#2297,.T.);
#1527=FACE_OUTER_BOUND('',#2303,.T.);
#1528=FACE_OUTER_BOUND('',#2304,.T.);
#1529=FACE_OUTER_BOUND('',#2310,.T.);
#1530=FACE_OUTER_BOUND('',#2311,.T.);
#1531=FACE_OUTER_BOUND('',#2312,.T.);
#1532=FACE_OUTER_BOUND('',#2315,.T.);
#1533=FACE_OUTER_BOUND('',#2316,.T.);
#1534=FACE_OUTER_BOUND('',#2317,.T.);
#1535=FACE_OUTER_BOUND('',#2318,.T.);
#1536=FACE_OUTER_BOUND('',#2319,.T.);
#1537=FACE_OUTER_BOUND('',#2320,.T.);
#1538=FACE_OUTER_BOUND('',#2322,.T.);
#1539=FACE_OUTER_BOUND('',#2323,.T.);
#1540=FACE_OUTER_BOUND('',#2324,.T.);
#1541=FACE_OUTER_BOUND('',#2330,.T.);
#1542=FACE_OUTER_BOUND('',#2336,.T.);
#1543=FACE_OUTER_BOUND('',#2337,.T.);
#1544=FACE_OUTER_BOUND('',#2338,.T.);
#1545=FACE_OUTER_BOUND('',#2339,.T.);
#1546=FACE_OUTER_BOUND('',#2340,.T.);
#1547=FACE_OUTER_BOUND('',#2341,.T.);
#1548=FACE_OUTER_BOUND('',#2343,.T.);
#1549=FACE_OUTER_BOUND('',#2344,.T.);
#1550=FACE_OUTER_BOUND('',#2345,.T.);
#1551=FACE_OUTER_BOUND('',#2351,.T.);
#1552=FACE_OUTER_BOUND('',#2357,.T.);
#1553=FACE_OUTER_BOUND('',#2358,.T.);
#1554=FACE_OUTER_BOUND('',#2359,.T.);
#1555=FACE_OUTER_BOUND('',#2360,.T.);
#1556=FACE_OUTER_BOUND('',#2361,.T.);
#1557=FACE_OUTER_BOUND('',#2362,.T.);
#1558=FACE_OUTER_BOUND('',#2363,.T.);
#1559=FACE_OUTER_BOUND('',#2364,.T.);
#1560=FACE_OUTER_BOUND('',#2365,.T.);
#1561=FACE_OUTER_BOUND('',#2367,.T.);
#1562=FACE_OUTER_BOUND('',#2368,.T.);
#1563=FACE_OUTER_BOUND('',#2370,.T.);
#1564=FACE_OUTER_BOUND('',#2371,.T.);
#1565=FACE_OUTER_BOUND('',#2372,.T.);
#1566=FACE_OUTER_BOUND('',#2373,.T.);
#1567=FACE_OUTER_BOUND('',#2375,.T.);
#1568=FACE_OUTER_BOUND('',#2376,.T.);
#1569=FACE_OUTER_BOUND('',#2377,.T.);
#1570=FACE_OUTER_BOUND('',#2378,.T.);
#1571=FACE_OUTER_BOUND('',#2380,.T.);
#1572=FACE_OUTER_BOUND('',#2381,.T.);
#1573=FACE_OUTER_BOUND('',#2382,.T.);
#1574=FACE_OUTER_BOUND('',#2383,.T.);
#1575=FACE_OUTER_BOUND('',#2384,.T.);
#1576=FACE_OUTER_BOUND('',#2385,.T.);
#1577=FACE_OUTER_BOUND('',#2386,.T.);
#1578=FACE_OUTER_BOUND('',#2387,.T.);
#1579=FACE_OUTER_BOUND('',#2388,.T.);
#1580=FACE_OUTER_BOUND('',#2389,.T.);
#1581=FACE_OUTER_BOUND('',#2390,.T.);
#1582=FACE_OUTER_BOUND('',#2391,.T.);
#1583=FACE_OUTER_BOUND('',#2392,.T.);
#1584=FACE_OUTER_BOUND('',#2393,.T.);
#1585=FACE_OUTER_BOUND('',#2394,.T.);
#1586=FACE_OUTER_BOUND('',#2395,.T.);
#1587=FACE_OUTER_BOUND('',#2396,.T.);
#1588=FACE_OUTER_BOUND('',#2397,.T.);
#1589=FACE_OUTER_BOUND('',#2398,.T.);
#1590=FACE_OUTER_BOUND('',#2399,.T.);
#1591=FACE_OUTER_BOUND('',#2400,.T.);
#1592=FACE_OUTER_BOUND('',#2401,.T.);
#1593=FACE_OUTER_BOUND('',#2402,.T.);
#1594=FACE_OUTER_BOUND('',#2403,.T.);
#1595=FACE_OUTER_BOUND('',#2405,.T.);
#1596=FACE_OUTER_BOUND('',#2406,.T.);
#1597=FACE_OUTER_BOUND('',#2408,.T.);
#1598=FACE_OUTER_BOUND('',#2409,.T.);
#1599=FACE_OUTER_BOUND('',#2411,.T.);
#1600=FACE_OUTER_BOUND('',#2412,.T.);
#1601=FACE_OUTER_BOUND('',#2414,.T.);
#1602=FACE_OUTER_BOUND('',#2415,.T.);
#1603=FACE_OUTER_BOUND('',#2417,.T.);
#1604=FACE_OUTER_BOUND('',#2418,.T.);
#1605=FACE_OUTER_BOUND('',#2419,.T.);
#1606=FACE_OUTER_BOUND('',#2420,.T.);
#1607=FACE_OUTER_BOUND('',#2421,.T.);
#1608=FACE_OUTER_BOUND('',#2422,.T.);
#1609=FACE_OUTER_BOUND('',#2423,.T.);
#1610=FACE_OUTER_BOUND('',#2424,.T.);
#1611=FACE_OUTER_BOUND('',#2425,.T.);
#1612=FACE_OUTER_BOUND('',#2426,.T.);
#1613=FACE_OUTER_BOUND('',#2427,.T.);
#1614=FACE_OUTER_BOUND('',#2428,.T.);
#1615=FACE_OUTER_BOUND('',#2429,.T.);
#1616=FACE_OUTER_BOUND('',#2430,.T.);
#1617=FACE_OUTER_BOUND('',#2431,.T.);
#1618=FACE_OUTER_BOUND('',#2433,.T.);
#1619=FACE_OUTER_BOUND('',#2434,.T.);
#1620=FACE_OUTER_BOUND('',#2435,.T.);
#1621=FACE_OUTER_BOUND('',#2436,.T.);
#1622=FACE_OUTER_BOUND('',#2437,.T.);
#1623=FACE_OUTER_BOUND('',#2438,.T.);
#1624=FACE_OUTER_BOUND('',#2439,.T.);
#1625=FACE_OUTER_BOUND('',#2440,.T.);
#1626=FACE_OUTER_BOUND('',#2441,.T.);
#1627=FACE_OUTER_BOUND('',#2442,.T.);
#1628=FACE_OUTER_BOUND('',#2443,.T.);
#1629=FACE_OUTER_BOUND('',#2444,.T.);
#1630=FACE_OUTER_BOUND('',#2445,.T.);
#1631=FACE_OUTER_BOUND('',#2446,.T.);
#1632=FACE_OUTER_BOUND('',#2447,.T.);
#1633=FACE_OUTER_BOUND('',#2448,.T.);
#1634=FACE_OUTER_BOUND('',#2449,.T.);
#1635=FACE_OUTER_BOUND('',#2450,.T.);
#1636=FACE_OUTER_BOUND('',#2451,.T.);
#1637=FACE_OUTER_BOUND('',#2452,.T.);
#1638=FACE_OUTER_BOUND('',#2453,.T.);
#1639=FACE_OUTER_BOUND('',#2454,.T.);
#1640=FACE_OUTER_BOUND('',#2455,.T.);
#1641=FACE_OUTER_BOUND('',#2456,.T.);
#1642=FACE_OUTER_BOUND('',#2457,.T.);
#1643=FACE_OUTER_BOUND('',#2458,.T.);
#1644=FACE_OUTER_BOUND('',#2459,.T.);
#1645=FACE_OUTER_BOUND('',#2460,.T.);
#1646=FACE_OUTER_BOUND('',#2461,.T.);
#1647=FACE_OUTER_BOUND('',#2462,.T.);
#1648=FACE_OUTER_BOUND('',#2463,.T.);
#1649=FACE_OUTER_BOUND('',#2464,.T.);
#1650=FACE_OUTER_BOUND('',#2465,.T.);
#1651=FACE_OUTER_BOUND('',#2466,.T.);
#1652=FACE_OUTER_BOUND('',#2467,.T.);
#1653=FACE_OUTER_BOUND('',#2468,.T.);
#1654=FACE_OUTER_BOUND('',#2469,.T.);
#1655=FACE_OUTER_BOUND('',#2470,.T.);
#1656=FACE_OUTER_BOUND('',#2471,.T.);
#1657=FACE_OUTER_BOUND('',#2472,.T.);
#1658=FACE_OUTER_BOUND('',#2473,.T.);
#1659=FACE_OUTER_BOUND('',#2474,.T.);
#1660=FACE_OUTER_BOUND('',#2475,.T.);
#1661=FACE_OUTER_BOUND('',#2476,.T.);
#1662=FACE_OUTER_BOUND('',#2477,.T.);
#1663=FACE_OUTER_BOUND('',#2478,.T.);
#1664=FACE_OUTER_BOUND('',#2479,.T.);
#1665=FACE_OUTER_BOUND('',#2480,.T.);
#1666=FACE_OUTER_BOUND('',#2481,.T.);
#1667=FACE_OUTER_BOUND('',#2482,.T.);
#1668=FACE_OUTER_BOUND('',#2483,.T.);
#1669=FACE_OUTER_BOUND('',#2484,.T.);
#1670=FACE_OUTER_BOUND('',#2485,.T.);
#1671=FACE_OUTER_BOUND('',#2486,.T.);
#1672=FACE_OUTER_BOUND('',#2487,.T.);
#1673=FACE_OUTER_BOUND('',#2488,.T.);
#1674=FACE_OUTER_BOUND('',#2489,.T.);
#1675=FACE_OUTER_BOUND('',#2490,.T.);
#1676=FACE_OUTER_BOUND('',#2491,.T.);
#1677=FACE_OUTER_BOUND('',#2492,.T.);
#1678=FACE_OUTER_BOUND('',#2493,.T.);
#1679=FACE_OUTER_BOUND('',#2494,.T.);
#1680=FACE_OUTER_BOUND('',#2495,.T.);
#1681=FACE_OUTER_BOUND('',#2496,.T.);
#1682=FACE_OUTER_BOUND('',#2497,.T.);
#1683=FACE_OUTER_BOUND('',#2498,.T.);
#1684=FACE_OUTER_BOUND('',#2499,.T.);
#1685=FACE_OUTER_BOUND('',#2500,.T.);
#1686=FACE_OUTER_BOUND('',#2501,.T.);
#1687=FACE_OUTER_BOUND('',#2502,.T.);
#1688=FACE_OUTER_BOUND('',#2503,.T.);
#1689=FACE_OUTER_BOUND('',#2504,.T.);
#1690=FACE_OUTER_BOUND('',#2505,.T.);
#1691=FACE_OUTER_BOUND('',#2506,.T.);
#1692=FACE_OUTER_BOUND('',#2507,.T.);
#1693=FACE_OUTER_BOUND('',#2508,.T.);
#1694=FACE_OUTER_BOUND('',#2509,.T.);
#1695=FACE_OUTER_BOUND('',#2510,.T.);
#1696=FACE_OUTER_BOUND('',#2511,.T.);
#1697=FACE_OUTER_BOUND('',#2512,.T.);
#1698=FACE_OUTER_BOUND('',#2513,.T.);
#1699=FACE_OUTER_BOUND('',#2514,.T.);
#1700=FACE_OUTER_BOUND('',#2515,.T.);
#1701=FACE_OUTER_BOUND('',#2516,.T.);
#1702=FACE_OUTER_BOUND('',#2517,.T.);
#1703=FACE_OUTER_BOUND('',#2518,.T.);
#1704=FACE_OUTER_BOUND('',#2519,.T.);
#1705=FACE_OUTER_BOUND('',#2520,.T.);
#1706=FACE_OUTER_BOUND('',#2521,.T.);
#1707=FACE_OUTER_BOUND('',#2522,.T.);
#1708=FACE_OUTER_BOUND('',#2523,.T.);
#1709=FACE_OUTER_BOUND('',#2524,.T.);
#1710=FACE_OUTER_BOUND('',#2525,.T.);
#1711=FACE_OUTER_BOUND('',#2526,.T.);
#1712=FACE_OUTER_BOUND('',#2527,.T.);
#1713=FACE_OUTER_BOUND('',#2528,.T.);
#1714=FACE_OUTER_BOUND('',#2529,.T.);
#1715=FACE_OUTER_BOUND('',#2530,.T.);
#1716=FACE_OUTER_BOUND('',#2531,.T.);
#1717=FACE_OUTER_BOUND('',#2532,.T.);
#1718=FACE_OUTER_BOUND('',#2533,.T.);
#1719=FACE_OUTER_BOUND('',#2534,.T.);
#1720=FACE_OUTER_BOUND('',#2535,.T.);
#1721=FACE_OUTER_BOUND('',#2536,.T.);
#1722=FACE_OUTER_BOUND('',#2537,.T.);
#1723=FACE_OUTER_BOUND('',#2538,.T.);
#1724=FACE_OUTER_BOUND('',#2539,.T.);
#1725=FACE_OUTER_BOUND('',#2540,.T.);
#1726=FACE_OUTER_BOUND('',#2541,.T.);
#1727=FACE_OUTER_BOUND('',#2542,.T.);
#1728=FACE_OUTER_BOUND('',#2543,.T.);
#1729=FACE_OUTER_BOUND('',#2544,.T.);
#1730=FACE_OUTER_BOUND('',#2545,.T.);
#1731=FACE_OUTER_BOUND('',#2546,.T.);
#1732=FACE_OUTER_BOUND('',#2547,.T.);
#1733=FACE_OUTER_BOUND('',#2548,.T.);
#1734=FACE_OUTER_BOUND('',#2549,.T.);
#1735=FACE_OUTER_BOUND('',#2550,.T.);
#1736=FACE_OUTER_BOUND('',#2551,.T.);
#1737=FACE_OUTER_BOUND('',#2552,.T.);
#1738=FACE_OUTER_BOUND('',#2553,.T.);
#1739=FACE_OUTER_BOUND('',#2554,.T.);
#1740=FACE_OUTER_BOUND('',#2555,.T.);
#1741=FACE_OUTER_BOUND('',#2556,.T.);
#1742=FACE_OUTER_BOUND('',#2557,.T.);
#1743=FACE_OUTER_BOUND('',#2558,.T.);
#1744=FACE_OUTER_BOUND('',#2559,.T.);
#1745=FACE_OUTER_BOUND('',#2560,.T.);
#1746=FACE_OUTER_BOUND('',#2561,.T.);
#1747=FACE_OUTER_BOUND('',#2562,.T.);
#1748=FACE_OUTER_BOUND('',#2563,.T.);
#1749=FACE_OUTER_BOUND('',#2564,.T.);
#1750=FACE_OUTER_BOUND('',#2565,.T.);
#1751=FACE_OUTER_BOUND('',#2566,.T.);
#1752=FACE_OUTER_BOUND('',#2567,.T.);
#1753=FACE_OUTER_BOUND('',#2568,.T.);
#1754=FACE_OUTER_BOUND('',#2569,.T.);
#1755=FACE_OUTER_BOUND('',#2570,.T.);
#1756=FACE_OUTER_BOUND('',#2571,.T.);
#1757=FACE_OUTER_BOUND('',#2572,.T.);
#1758=FACE_OUTER_BOUND('',#2573,.T.);
#1759=FACE_OUTER_BOUND('',#2574,.T.);
#1760=FACE_OUTER_BOUND('',#2575,.T.);
#1761=FACE_OUTER_BOUND('',#2576,.T.);
#1762=FACE_OUTER_BOUND('',#2577,.T.);
#1763=FACE_OUTER_BOUND('',#2578,.T.);
#1764=FACE_OUTER_BOUND('',#2579,.T.);
#1765=FACE_OUTER_BOUND('',#2580,.T.);
#1766=FACE_OUTER_BOUND('',#2581,.T.);
#1767=FACE_OUTER_BOUND('',#2582,.T.);
#1768=FACE_OUTER_BOUND('',#2583,.T.);
#1769=FACE_OUTER_BOUND('',#2584,.T.);
#1770=FACE_OUTER_BOUND('',#2585,.T.);
#1771=FACE_OUTER_BOUND('',#2586,.T.);
#1772=FACE_OUTER_BOUND('',#2587,.T.);
#1773=FACE_OUTER_BOUND('',#2588,.T.);
#1774=FACE_OUTER_BOUND('',#2589,.T.);
#1775=FACE_OUTER_BOUND('',#2590,.T.);
#1776=FACE_OUTER_BOUND('',#2591,.T.);
#1777=FACE_OUTER_BOUND('',#2592,.T.);
#1778=FACE_OUTER_BOUND('',#2593,.T.);
#1779=FACE_OUTER_BOUND('',#2594,.T.);
#1780=FACE_OUTER_BOUND('',#2595,.T.);
#1781=FACE_OUTER_BOUND('',#2596,.T.);
#1782=FACE_OUTER_BOUND('',#2597,.T.);
#1783=FACE_OUTER_BOUND('',#2598,.T.);
#1784=FACE_OUTER_BOUND('',#2599,.T.);
#1785=FACE_OUTER_BOUND('',#2600,.T.);
#1786=FACE_OUTER_BOUND('',#2601,.T.);
#1787=FACE_OUTER_BOUND('',#2602,.T.);
#1788=FACE_OUTER_BOUND('',#2603,.T.);
#1789=FACE_OUTER_BOUND('',#2604,.T.);
#1790=FACE_OUTER_BOUND('',#2605,.T.);
#1791=FACE_OUTER_BOUND('',#2606,.T.);
#1792=FACE_OUTER_BOUND('',#2608,.T.);
#1793=FACE_OUTER_BOUND('',#2609,.T.);
#1794=FACE_OUTER_BOUND('',#2610,.T.);
#1795=FACE_OUTER_BOUND('',#2611,.T.);
#1796=FACE_OUTER_BOUND('',#2613,.T.);
#1797=FACE_OUTER_BOUND('',#2614,.T.);
#1798=FACE_OUTER_BOUND('',#2616,.T.);
#1799=FACE_OUTER_BOUND('',#2618,.T.);
#1800=FACE_OUTER_BOUND('',#2620,.T.);
#1801=FACE_OUTER_BOUND('',#2622,.T.);
#1802=FACE_OUTER_BOUND('',#2623,.T.);
#1803=FACE_OUTER_BOUND('',#2624,.T.);
#1804=FACE_OUTER_BOUND('',#2625,.T.);
#1805=FACE_OUTER_BOUND('',#2626,.T.);
#1806=FACE_OUTER_BOUND('',#2627,.T.);
#1807=FACE_OUTER_BOUND('',#2628,.T.);
#1808=FACE_OUTER_BOUND('',#2629,.T.);
#1809=FACE_OUTER_BOUND('',#2630,.T.);
#1810=FACE_OUTER_BOUND('',#2631,.T.);
#1811=FACE_OUTER_BOUND('',#2632,.T.);
#1812=FACE_OUTER_BOUND('',#2633,.T.);
#1813=FACE_OUTER_BOUND('',#2634,.T.);
#1814=FACE_OUTER_BOUND('',#2636,.T.);
#1815=FACE_OUTER_BOUND('',#2638,.T.);
#1816=FACE_OUTER_BOUND('',#2639,.T.);
#1817=FACE_OUTER_BOUND('',#2640,.T.);
#1818=FACE_OUTER_BOUND('',#2641,.T.);
#1819=FACE_OUTER_BOUND('',#2642,.T.);
#1820=FACE_OUTER_BOUND('',#2643,.T.);
#1821=FACE_OUTER_BOUND('',#2644,.T.);
#1822=FACE_OUTER_BOUND('',#2645,.T.);
#1823=FACE_OUTER_BOUND('',#2646,.T.);
#1824=FACE_OUTER_BOUND('',#2648,.T.);
#1825=FACE_OUTER_BOUND('',#2649,.T.);
#1826=FACE_OUTER_BOUND('',#2650,.T.);
#1827=FACE_OUTER_BOUND('',#2651,.T.);
#1828=FACE_OUTER_BOUND('',#2652,.T.);
#1829=FACE_OUTER_BOUND('',#2653,.T.);
#1830=FACE_OUTER_BOUND('',#2654,.T.);
#1831=FACE_OUTER_BOUND('',#2655,.T.);
#1832=FACE_OUTER_BOUND('',#2656,.T.);
#1833=FACE_OUTER_BOUND('',#2657,.T.);
#1834=FACE_OUTER_BOUND('',#2658,.T.);
#1835=FACE_OUTER_BOUND('',#2659,.T.);
#1836=FACE_OUTER_BOUND('',#2660,.T.);
#1837=FACE_OUTER_BOUND('',#2661,.T.);
#1838=FACE_OUTER_BOUND('',#2662,.T.);
#1839=FACE_OUTER_BOUND('',#2663,.T.);
#1840=FACE_OUTER_BOUND('',#2664,.T.);
#1841=FACE_OUTER_BOUND('',#2665,.T.);
#1842=FACE_OUTER_BOUND('',#2666,.T.);
#1843=FACE_OUTER_BOUND('',#2669,.T.);
#1844=FACE_OUTER_BOUND('',#2671,.T.);
#1845=FACE_OUTER_BOUND('',#2673,.T.);
#1846=FACE_OUTER_BOUND('',#2674,.T.);
#1847=FACE_OUTER_BOUND('',#2675,.T.);
#1848=FACE_OUTER_BOUND('',#2677,.T.);
#1849=FACE_OUTER_BOUND('',#2679,.T.);
#1850=FACE_OUTER_BOUND('',#2680,.T.);
#1851=FACE_OUTER_BOUND('',#2681,.T.);
#1852=FACE_OUTER_BOUND('',#2683,.T.);
#1853=FACE_OUTER_BOUND('',#2685,.T.);
#1854=FACE_OUTER_BOUND('',#2686,.T.);
#1855=FACE_OUTER_BOUND('',#2687,.T.);
#1856=FACE_OUTER_BOUND('',#2689,.T.);
#1857=FACE_OUTER_BOUND('',#2691,.T.);
#1858=FACE_OUTER_BOUND('',#2692,.T.);
#1859=FACE_OUTER_BOUND('',#2693,.T.);
#1860=FACE_OUTER_BOUND('',#2695,.T.);
#1861=FACE_OUTER_BOUND('',#2697,.T.);
#1862=FACE_OUTER_BOUND('',#2698,.T.);
#1863=FACE_OUTER_BOUND('',#2699,.T.);
#1864=FACE_OUTER_BOUND('',#2700,.T.);
#1865=FACE_OUTER_BOUND('',#2701,.T.);
#1866=FACE_OUTER_BOUND('',#2702,.T.);
#1867=FACE_OUTER_BOUND('',#2703,.T.);
#1868=FACE_OUTER_BOUND('',#2704,.T.);
#1869=FACE_OUTER_BOUND('',#2705,.T.);
#1870=FACE_OUTER_BOUND('',#2706,.T.);
#1871=FACE_OUTER_BOUND('',#2707,.T.);
#1872=FACE_OUTER_BOUND('',#2708,.T.);
#1873=FACE_OUTER_BOUND('',#2709,.T.);
#1874=FACE_OUTER_BOUND('',#2710,.T.);
#1875=FACE_OUTER_BOUND('',#2711,.T.);
#1876=FACE_OUTER_BOUND('',#2712,.T.);
#1877=FACE_OUTER_BOUND('',#2713,.T.);
#1878=FACE_OUTER_BOUND('',#2715,.T.);
#1879=FACE_OUTER_BOUND('',#2716,.T.);
#1880=FACE_OUTER_BOUND('',#2717,.T.);
#1881=FACE_OUTER_BOUND('',#2718,.T.);
#1882=FACE_OUTER_BOUND('',#2720,.T.);
#1883=FACE_OUTER_BOUND('',#2721,.T.);
#1884=FACE_OUTER_BOUND('',#2723,.T.);
#1885=FACE_OUTER_BOUND('',#2725,.T.);
#1886=FACE_OUTER_BOUND('',#2727,.T.);
#1887=FACE_OUTER_BOUND('',#2728,.T.);
#1888=FACE_OUTER_BOUND('',#2729,.T.);
#1889=FACE_OUTER_BOUND('',#2731,.T.);
#1890=FACE_OUTER_BOUND('',#2733,.T.);
#1891=FACE_OUTER_BOUND('',#2734,.T.);
#1892=FACE_OUTER_BOUND('',#2735,.T.);
#1893=FACE_OUTER_BOUND('',#2737,.T.);
#1894=FACE_OUTER_BOUND('',#2739,.T.);
#1895=FACE_OUTER_BOUND('',#2740,.T.);
#1896=FACE_OUTER_BOUND('',#2741,.T.);
#1897=FACE_OUTER_BOUND('',#2743,.T.);
#1898=FACE_OUTER_BOUND('',#2745,.T.);
#1899=FACE_OUTER_BOUND('',#2746,.T.);
#1900=FACE_OUTER_BOUND('',#2747,.T.);
#1901=FACE_OUTER_BOUND('',#2748,.T.);
#1902=FACE_OUTER_BOUND('',#2750,.T.);
#1903=FACE_OUTER_BOUND('',#2751,.T.);
#1904=FACE_OUTER_BOUND('',#2752,.T.);
#1905=FACE_OUTER_BOUND('',#2754,.T.);
#1906=FACE_OUTER_BOUND('',#2755,.T.);
#1907=FACE_OUTER_BOUND('',#2756,.T.);
#1908=FACE_OUTER_BOUND('',#2757,.T.);
#1909=FACE_OUTER_BOUND('',#2758,.T.);
#1910=FACE_OUTER_BOUND('',#2759,.T.);
#1911=FACE_OUTER_BOUND('',#2760,.T.);
#1912=FACE_OUTER_BOUND('',#2761,.T.);
#1913=FACE_OUTER_BOUND('',#2762,.T.);
#1914=FACE_OUTER_BOUND('',#2763,.T.);
#1915=FACE_OUTER_BOUND('',#2764,.T.);
#1916=FACE_OUTER_BOUND('',#2765,.T.);
#1917=FACE_OUTER_BOUND('',#2766,.T.);
#1918=FACE_OUTER_BOUND('',#2767,.T.);
#1919=FACE_OUTER_BOUND('',#2768,.T.);
#1920=FACE_OUTER_BOUND('',#2769,.T.);
#1921=FACE_OUTER_BOUND('',#2770,.T.);
#1922=FACE_OUTER_BOUND('',#2771,.T.);
#1923=FACE_OUTER_BOUND('',#2772,.T.);
#1924=FACE_OUTER_BOUND('',#2773,.T.);
#1925=FACE_OUTER_BOUND('',#2774,.T.);
#1926=FACE_OUTER_BOUND('',#2775,.T.);
#1927=FACE_OUTER_BOUND('',#2776,.T.);
#1928=FACE_OUTER_BOUND('',#2777,.T.);
#1929=FACE_OUTER_BOUND('',#2778,.T.);
#1930=FACE_OUTER_BOUND('',#2779,.T.);
#1931=FACE_OUTER_BOUND('',#2780,.T.);
#1932=FACE_OUTER_BOUND('',#2781,.T.);
#1933=FACE_OUTER_BOUND('',#2782,.T.);
#1934=FACE_OUTER_BOUND('',#2783,.T.);
#1935=FACE_OUTER_BOUND('',#2784,.T.);
#1936=FACE_OUTER_BOUND('',#2785,.T.);
#1937=FACE_OUTER_BOUND('',#2786,.T.);
#1938=FACE_OUTER_BOUND('',#2787,.T.);
#1939=FACE_OUTER_BOUND('',#2788,.T.);
#1940=FACE_OUTER_BOUND('',#2789,.T.);
#1941=FACE_OUTER_BOUND('',#2790,.T.);
#1942=FACE_OUTER_BOUND('',#2791,.T.);
#1943=FACE_OUTER_BOUND('',#2792,.T.);
#1944=FACE_OUTER_BOUND('',#2793,.T.);
#1945=FACE_OUTER_BOUND('',#2794,.T.);
#1946=FACE_OUTER_BOUND('',#2795,.T.);
#1947=FACE_OUTER_BOUND('',#2796,.T.);
#1948=FACE_OUTER_BOUND('',#2797,.T.);
#1949=FACE_OUTER_BOUND('',#2798,.T.);
#1950=FACE_OUTER_BOUND('',#2799,.T.);
#1951=FACE_OUTER_BOUND('',#2800,.T.);
#1952=FACE_OUTER_BOUND('',#2801,.T.);
#1953=FACE_OUTER_BOUND('',#2802,.T.);
#1954=FACE_OUTER_BOUND('',#2803,.T.);
#1955=FACE_OUTER_BOUND('',#2804,.T.);
#1956=FACE_OUTER_BOUND('',#2805,.T.);
#1957=FACE_OUTER_BOUND('',#2806,.T.);
#1958=FACE_OUTER_BOUND('',#2807,.T.);
#1959=FACE_OUTER_BOUND('',#2808,.T.);
#1960=FACE_OUTER_BOUND('',#2809,.T.);
#1961=FACE_OUTER_BOUND('',#2810,.T.);
#1962=FACE_OUTER_BOUND('',#2811,.T.);
#1963=FACE_OUTER_BOUND('',#2812,.T.);
#1964=FACE_OUTER_BOUND('',#2813,.T.);
#1965=FACE_OUTER_BOUND('',#2814,.T.);
#1966=FACE_OUTER_BOUND('',#2815,.T.);
#1967=FACE_OUTER_BOUND('',#2816,.T.);
#1968=FACE_OUTER_BOUND('',#2817,.T.);
#1969=FACE_OUTER_BOUND('',#2818,.T.);
#1970=FACE_OUTER_BOUND('',#2819,.T.);
#1971=FACE_OUTER_BOUND('',#2820,.T.);
#1972=FACE_OUTER_BOUND('',#2821,.T.);
#1973=FACE_OUTER_BOUND('',#2822,.T.);
#1974=FACE_OUTER_BOUND('',#2823,.T.);
#1975=FACE_OUTER_BOUND('',#2824,.T.);
#1976=FACE_OUTER_BOUND('',#2825,.T.);
#1977=FACE_OUTER_BOUND('',#2826,.T.);
#1978=FACE_OUTER_BOUND('',#2827,.T.);
#1979=FACE_OUTER_BOUND('',#2828,.T.);
#1980=FACE_OUTER_BOUND('',#2829,.T.);
#1981=FACE_OUTER_BOUND('',#2830,.T.);
#1982=FACE_OUTER_BOUND('',#2831,.T.);
#1983=FACE_OUTER_BOUND('',#2832,.T.);
#1984=FACE_OUTER_BOUND('',#2833,.T.);
#1985=FACE_OUTER_BOUND('',#2835,.T.);
#1986=FACE_OUTER_BOUND('',#2836,.T.);
#1987=FACE_OUTER_BOUND('',#2837,.T.);
#1988=FACE_OUTER_BOUND('',#2838,.T.);
#1989=FACE_OUTER_BOUND('',#2840,.T.);
#1990=FACE_OUTER_BOUND('',#2842,.T.);
#1991=FACE_OUTER_BOUND('',#2843,.T.);
#1992=FACE_OUTER_BOUND('',#2844,.T.);
#1993=FACE_OUTER_BOUND('',#2845,.T.);
#1994=FACE_OUTER_BOUND('',#2846,.T.);
#1995=FACE_OUTER_BOUND('',#2848,.T.);
#1996=FACE_OUTER_BOUND('',#2849,.T.);
#1997=FACE_OUTER_BOUND('',#2850,.T.);
#1998=FACE_OUTER_BOUND('',#2851,.T.);
#1999=FACE_OUTER_BOUND('',#2852,.T.);
#2000=FACE_OUTER_BOUND('',#2853,.T.);
#2001=FACE_OUTER_BOUND('',#2854,.T.);
#2002=FACE_OUTER_BOUND('',#2855,.T.);
#2003=FACE_OUTER_BOUND('',#2856,.T.);
#2004=FACE_OUTER_BOUND('',#2857,.T.);
#2005=FACE_OUTER_BOUND('',#2858,.T.);
#2006=FACE_OUTER_BOUND('',#2859,.T.);
#2007=FACE_OUTER_BOUND('',#2860,.T.);
#2008=FACE_OUTER_BOUND('',#2861,.T.);
#2009=FACE_OUTER_BOUND('',#2862,.T.);
#2010=FACE_OUTER_BOUND('',#2863,.T.);
#2011=FACE_OUTER_BOUND('',#2864,.T.);
#2012=FACE_OUTER_BOUND('',#2866,.T.);
#2013=FACE_OUTER_BOUND('',#2867,.T.);
#2014=FACE_OUTER_BOUND('',#2868,.T.);
#2015=FACE_OUTER_BOUND('',#2869,.T.);
#2016=FACE_OUTER_BOUND('',#2870,.T.);
#2017=FACE_OUTER_BOUND('',#2871,.T.);
#2018=FACE_OUTER_BOUND('',#2872,.T.);
#2019=FACE_OUTER_BOUND('',#2873,.T.);
#2020=FACE_OUTER_BOUND('',#2874,.T.);
#2021=FACE_OUTER_BOUND('',#2875,.T.);
#2022=FACE_OUTER_BOUND('',#2876,.T.);
#2023=FACE_OUTER_BOUND('',#2877,.T.);
#2024=FACE_OUTER_BOUND('',#2878,.T.);
#2025=FACE_OUTER_BOUND('',#2879,.T.);
#2026=FACE_OUTER_BOUND('',#2880,.T.);
#2027=FACE_OUTER_BOUND('',#2882,.T.);
#2028=EDGE_LOOP('',(#8421,#8422,#8423,#8424));
#2029=EDGE_LOOP('',(#8425,#8426,#8427,#8428));
#2030=EDGE_LOOP('',(#8429,#8430,#8431,#8432));
#2031=EDGE_LOOP('',(#8433,#8434,#8435,#8436));
#2032=EDGE_LOOP('',(#8437,#8438,#8439,#8440));
#2033=EDGE_LOOP('',(#8441,#8442,#8443,#8444));
#2034=EDGE_LOOP('',(#8445,#8446,#8447,#8448));
#2035=EDGE_LOOP('',(#8449,#8450,#8451,#8452));
#2036=EDGE_LOOP('',(#8453,#8454,#8455,#8456));
#2037=EDGE_LOOP('',(#8457,#8458,#8459,#8460));
#2038=EDGE_LOOP('',(#8461,#8462,#8463,#8464));
#2039=EDGE_LOOP('',(#8465));
#2040=EDGE_LOOP('',(#8466));
#2041=EDGE_LOOP('',(#8467));
#2042=EDGE_LOOP('',(#8468));
#2043=EDGE_LOOP('',(#8469));
#2044=EDGE_LOOP('',(#8470));
#2045=EDGE_LOOP('',(#8471,#8472,#8473,#8474));
#2046=EDGE_LOOP('',(#8475));
#2047=EDGE_LOOP('',(#8476));
#2048=EDGE_LOOP('',(#8477));
#2049=EDGE_LOOP('',(#8478));
#2050=EDGE_LOOP('',(#8479));
#2051=EDGE_LOOP('',(#8480));
#2052=EDGE_LOOP('',(#8481,#8482,#8483,#8484));
#2053=EDGE_LOOP('',(#8485,#8486,#8487,#8488));
#2054=EDGE_LOOP('',(#8489,#8490,#8491,#8492));
#2055=EDGE_LOOP('',(#8493,#8494,#8495,#8496));
#2056=EDGE_LOOP('',(#8497,#8498,#8499,#8500));
#2057=EDGE_LOOP('',(#8501,#8502,#8503,#8504));
#2058=EDGE_LOOP('',(#8505,#8506,#8507,#8508));
#2059=EDGE_LOOP('',(#8509,#8510,#8511,#8512));
#2060=EDGE_LOOP('',(#8513,#8514,#8515,#8516));
#2061=EDGE_LOOP('',(#8517,#8518,#8519,#8520));
#2062=EDGE_LOOP('',(#8521,#8522,#8523,#8524));
#2063=EDGE_LOOP('',(#8525,#8526,#8527,#8528));
#2064=EDGE_LOOP('',(#8529,#8530,#8531,#8532));
#2065=EDGE_LOOP('',(#8533));
#2066=EDGE_LOOP('',(#8534,#8535,#8536,#8537));
#2067=EDGE_LOOP('',(#8538));
#2068=EDGE_LOOP('',(#8539,#8540,#8541,#8542));
#2069=EDGE_LOOP('',(#8543,#8544,#8545,#8546));
#2070=EDGE_LOOP('',(#8547,#8548,#8549,#8550,#8551,#8552,#8553,#8554));
#2071=EDGE_LOOP('',(#8555,#8556,#8557,#8558));
#2072=EDGE_LOOP('',(#8559,#8560,#8561,#8562));
#2073=EDGE_LOOP('',(#8563,#8564,#8565,#8566));
#2074=EDGE_LOOP('',(#8567,#8568,#8569,#8570,#8571,#8572,#8573,#8574));
#2075=EDGE_LOOP('',(#8575));
#2076=EDGE_LOOP('',(#8576));
#2077=EDGE_LOOP('',(#8577,#8578,#8579,#8580));
#2078=EDGE_LOOP('',(#8581,#8582,#8583,#8584));
#2079=EDGE_LOOP('',(#8585,#8586,#8587,#8588));
#2080=EDGE_LOOP('',(#8589));
#2081=EDGE_LOOP('',(#8590,#8591,#8592,#8593));
#2082=EDGE_LOOP('',(#8594));
#2083=EDGE_LOOP('',(#8595,#8596,#8597,#8598));
#2084=EDGE_LOOP('',(#8599,#8600,#8601,#8602));
#2085=EDGE_LOOP('',(#8603,#8604,#8605,#8606,#8607,#8608,#8609,#8610,#8611,
#8612,#8613,#8614,#8615,#8616,#8617));
#2086=EDGE_LOOP('',(#8618,#8619,#8620,#8621));
#2087=EDGE_LOOP('',(#8622,#8623,#8624,#8625));
#2088=EDGE_LOOP('',(#8626,#8627,#8628,#8629));
#2089=EDGE_LOOP('',(#8630,#8631,#8632,#8633,#8634,#8635,#8636,#8637));
#2090=EDGE_LOOP('',(#8638));
#2091=EDGE_LOOP('',(#8639));
#2092=EDGE_LOOP('',(#8640,#8641,#8642,#8643));
#2093=EDGE_LOOP('',(#8644,#8645,#8646,#8647));
#2094=EDGE_LOOP('',(#8648,#8649,#8650,#8651,#8652,#8653,#8654,#8655));
#2095=EDGE_LOOP('',(#8656,#8657,#8658,#8659));
#2096=EDGE_LOOP('',(#8660,#8661));
#2097=EDGE_LOOP('',(#8662,#8663,#8664,#8665,#8666,#8667,#8668,#8669,#8670));
#2098=EDGE_LOOP('',(#8671,#8672));
#2099=EDGE_LOOP('',(#8673,#8674));
#2100=EDGE_LOOP('',(#8675,#8676,#8677,#8678));
#2101=EDGE_LOOP('',(#8679,#8680,#8681,#8682,#8683));
#2102=EDGE_LOOP('',(#8684,#8685,#8686,#8687,#8688,#8689));
#2103=EDGE_LOOP('',(#8690,#8691));
#2104=EDGE_LOOP('',(#8692));
#2105=EDGE_LOOP('',(#8693));
#2106=EDGE_LOOP('',(#8694,#8695,#8696,#8697));
#2107=EDGE_LOOP('',(#8698,#8699,#8700,#8701,#8702,#8703));
#2108=EDGE_LOOP('',(#8704,#8705,#8706,#8707));
#2109=EDGE_LOOP('',(#8708,#8709,#8710,#8711));
#2110=EDGE_LOOP('',(#8712));
#2111=EDGE_LOOP('',(#8713,#8714,#8715,#8716));
#2112=EDGE_LOOP('',(#8717,#8718));
#2113=EDGE_LOOP('',(#8719,#8720,#8721,#8722));
#2114=EDGE_LOOP('',(#8723,#8724));
#2115=EDGE_LOOP('',(#8725));
#2116=EDGE_LOOP('',(#8726,#8727,#8728,#8729,#8730));
#2117=EDGE_LOOP('',(#8731));
#2118=EDGE_LOOP('',(#8732));
#2119=EDGE_LOOP('',(#8733,#8734));
#2120=EDGE_LOOP('',(#8735,#8736,#8737,#8738,#8739,#8740,#8741,#8742,#8743));
#2121=EDGE_LOOP('',(#8744,#8745));
#2122=EDGE_LOOP('',(#8746,#8747,#8748,#8749));
#2123=EDGE_LOOP('',(#8750,#8751,#8752,#8753));
#2124=EDGE_LOOP('',(#8754,#8755,#8756,#8757,#8758,#8759,#8760,#8761,#8762,
#8763,#8764,#8765));
#2125=EDGE_LOOP('',(#8766,#8767));
#2126=EDGE_LOOP('',(#8768));
#2127=EDGE_LOOP('',(#8769));
#2128=EDGE_LOOP('',(#8770,#8771,#8772,#8773));
#2129=EDGE_LOOP('',(#8774,#8775,#8776,#8777,#8778));
#2130=EDGE_LOOP('',(#8779,#8780,#8781,#8782));
#2131=EDGE_LOOP('',(#8783));
#2132=EDGE_LOOP('',(#8784));
#2133=EDGE_LOOP('',(#8785));
#2134=EDGE_LOOP('',(#8786));
#2135=EDGE_LOOP('',(#8787,#8788,#8789,#8790));
#2136=EDGE_LOOP('',(#8791,#8792,#8793,#8794));
#2137=EDGE_LOOP('',(#8795,#8796,#8797,#8798,#8799,#8800));
#2138=EDGE_LOOP('',(#8801,#8802,#8803,#8804,#8805,#8806));
#2139=EDGE_LOOP('',(#8807,#8808,#8809,#8810,#8811,#8812));
#2140=EDGE_LOOP('',(#8813,#8814,#8815,#8816));
#2141=EDGE_LOOP('',(#8817,#8818,#8819,#8820));
#2142=EDGE_LOOP('',(#8821,#8822,#8823,#8824));
#2143=EDGE_LOOP('',(#8825,#8826,#8827,#8828));
#2144=EDGE_LOOP('',(#8829,#8830,#8831,#8832,#8833,#8834));
#2145=EDGE_LOOP('',(#8835,#8836,#8837,#8838));
#2146=EDGE_LOOP('',(#8839,#8840,#8841,#8842));
#2147=EDGE_LOOP('',(#8843,#8844,#8845,#8846));
#2148=EDGE_LOOP('',(#8847,#8848,#8849,#8850));
#2149=EDGE_LOOP('',(#8851,#8852,#8853,#8854));
#2150=EDGE_LOOP('',(#8855,#8856,#8857,#8858));
#2151=EDGE_LOOP('',(#8859,#8860,#8861,#8862));
#2152=EDGE_LOOP('',(#8863,#8864,#8865,#8866));
#2153=EDGE_LOOP('',(#8867,#8868,#8869,#8870,#8871,#8872,#8873,#8874,#8875,
#8876));
#2154=EDGE_LOOP('',(#8877));
#2155=EDGE_LOOP('',(#8878));
#2156=EDGE_LOOP('',(#8879,#8880,#8881,#8882));
#2157=EDGE_LOOP('',(#8883,#8884,#8885,#8886));
#2158=EDGE_LOOP('',(#8887,#8888,#8889,#8890));
#2159=EDGE_LOOP('',(#8891,#8892,#8893,#8894));
#2160=EDGE_LOOP('',(#8895,#8896,#8897,#8898,#8899,#8900,#8901,#8902,#8903,
#8904));
#2161=EDGE_LOOP('',(#8905));
#2162=EDGE_LOOP('',(#8906));
#2163=EDGE_LOOP('',(#8907,#8908,#8909,#8910));
#2164=EDGE_LOOP('',(#8911,#8912,#8913,#8914));
#2165=EDGE_LOOP('',(#8915,#8916,#8917,#8918,#8919,#8920));
#2166=EDGE_LOOP('',(#8921,#8922,#8923,#8924,#8925,#8926));
#2167=EDGE_LOOP('',(#8927,#8928,#8929,#8930,#8931,#8932));
#2168=EDGE_LOOP('',(#8933,#8934,#8935,#8936));
#2169=EDGE_LOOP('',(#8937,#8938,#8939,#8940));
#2170=EDGE_LOOP('',(#8941,#8942,#8943,#8944));
#2171=EDGE_LOOP('',(#8945,#8946,#8947,#8948));
#2172=EDGE_LOOP('',(#8949,#8950,#8951,#8952,#8953,#8954));
#2173=EDGE_LOOP('',(#8955,#8956,#8957,#8958));
#2174=EDGE_LOOP('',(#8959,#8960,#8961,#8962));
#2175=EDGE_LOOP('',(#8963,#8964,#8965,#8966));
#2176=EDGE_LOOP('',(#8967,#8968,#8969,#8970));
#2177=EDGE_LOOP('',(#8971,#8972,#8973,#8974));
#2178=EDGE_LOOP('',(#8975,#8976,#8977,#8978));
#2179=EDGE_LOOP('',(#8979,#8980,#8981,#8982));
#2180=EDGE_LOOP('',(#8983,#8984,#8985,#8986));
#2181=EDGE_LOOP('',(#8987,#8988,#8989,#8990,#8991,#8992,#8993,#8994,#8995,
#8996));
#2182=EDGE_LOOP('',(#8997));
#2183=EDGE_LOOP('',(#8998));
#2184=EDGE_LOOP('',(#8999,#9000,#9001,#9002));
#2185=EDGE_LOOP('',(#9003,#9004,#9005,#9006));
#2186=EDGE_LOOP('',(#9007,#9008,#9009,#9010));
#2187=EDGE_LOOP('',(#9011,#9012,#9013,#9014));
#2188=EDGE_LOOP('',(#9015,#9016,#9017,#9018,#9019,#9020,#9021,#9022,#9023,
#9024));
#2189=EDGE_LOOP('',(#9025));
#2190=EDGE_LOOP('',(#9026));
#2191=EDGE_LOOP('',(#9027,#9028,#9029,#9030));
#2192=EDGE_LOOP('',(#9031,#9032,#9033,#9034));
#2193=EDGE_LOOP('',(#9035,#9036,#9037,#9038));
#2194=EDGE_LOOP('',(#9039));
#2195=EDGE_LOOP('',(#9040));
#2196=EDGE_LOOP('',(#9041,#9042,#9043,#9044));
#2197=EDGE_LOOP('',(#9045,#9046,#9047,#9048));
#2198=EDGE_LOOP('',(#9049,#9050,#9051,#9052));
#2199=EDGE_LOOP('',(#9053));
#2200=EDGE_LOOP('',(#9054));
#2201=EDGE_LOOP('',(#9055,#9056));
#2202=EDGE_LOOP('',(#9057,#9058,#9059,#9060,#9061,#9062,#9063,#9064,#9065));
#2203=EDGE_LOOP('',(#9066,#9067));
#2204=EDGE_LOOP('',(#9068,#9069,#9070,#9071));
#2205=EDGE_LOOP('',(#9072,#9073,#9074,#9075));
#2206=EDGE_LOOP('',(#9076,#9077,#9078,#9079,#9080));
#2207=EDGE_LOOP('',(#9081,#9082,#9083,#9084));
#2208=EDGE_LOOP('',(#9085,#9086));
#2209=EDGE_LOOP('',(#9087));
#2210=EDGE_LOOP('',(#9088));
#2211=EDGE_LOOP('',(#9089,#9090,#9091,#9092));
#2212=EDGE_LOOP('',(#9093,#9094,#9095,#9096));
#2213=EDGE_LOOP('',(#9097,#9098,#9099,#9100));
#2214=EDGE_LOOP('',(#9101,#9102,#9103,#9104));
#2215=EDGE_LOOP('',(#9105,#9106,#9107,#9108));
#2216=EDGE_LOOP('',(#9109,#9110,#9111,#9112));
#2217=EDGE_LOOP('',(#9113,#9114,#9115,#9116));
#2218=EDGE_LOOP('',(#9117,#9118,#9119,#9120));
#2219=EDGE_LOOP('',(#9121));
#2220=EDGE_LOOP('',(#9122,#9123,#9124,#9125));
#2221=EDGE_LOOP('',(#9126));
#2222=EDGE_LOOP('',(#9127,#9128,#9129,#9130));
#2223=EDGE_LOOP('',(#9131,#9132,#9133,#9134));
#2224=EDGE_LOOP('',(#9135,#9136,#9137,#9138,#9139,#9140,#9141,#9142));
#2225=EDGE_LOOP('',(#9143));
#2226=EDGE_LOOP('',(#9144));
#2227=EDGE_LOOP('',(#9145));
#2228=EDGE_LOOP('',(#9146));
#2229=EDGE_LOOP('',(#9147));
#2230=EDGE_LOOP('',(#9148,#9149,#9150,#9151));
#2231=EDGE_LOOP('',(#9152,#9153,#9154,#9155,#9156,#9157,#9158,#9159));
#2232=EDGE_LOOP('',(#9160));
#2233=EDGE_LOOP('',(#9161));
#2234=EDGE_LOOP('',(#9162));
#2235=EDGE_LOOP('',(#9163));
#2236=EDGE_LOOP('',(#9164));
#2237=EDGE_LOOP('',(#9165,#9166,#9167,#9168));
#2238=EDGE_LOOP('',(#9169,#9170,#9171,#9172));
#2239=EDGE_LOOP('',(#9173,#9174,#9175,#9176));
#2240=EDGE_LOOP('',(#9177));
#2241=EDGE_LOOP('',(#9178));
#2242=EDGE_LOOP('',(#9179,#9180,#9181,#9182));
#2243=EDGE_LOOP('',(#9183,#9184,#9185,#9186));
#2244=EDGE_LOOP('',(#9187,#9188,#9189,#9190));
#2245=EDGE_LOOP('',(#9191,#9192,#9193,#9194));
#2246=EDGE_LOOP('',(#9195,#9196,#9197,#9198));
#2247=EDGE_LOOP('',(#9199));
#2248=EDGE_LOOP('',(#9200));
#2249=EDGE_LOOP('',(#9201,#9202,#9203,#9204));
#2250=EDGE_LOOP('',(#9205,#9206,#9207,#9208));
#2251=EDGE_LOOP('',(#9209));
#2252=EDGE_LOOP('',(#9210));
#2253=EDGE_LOOP('',(#9211));
#2254=EDGE_LOOP('',(#9212));
#2255=EDGE_LOOP('',(#9213));
#2256=EDGE_LOOP('',(#9214));
#2257=EDGE_LOOP('',(#9215));
#2258=EDGE_LOOP('',(#9216));
#2259=EDGE_LOOP('',(#9217));
#2260=EDGE_LOOP('',(#9218));
#2261=EDGE_LOOP('',(#9219));
#2262=EDGE_LOOP('',(#9220));
#2263=EDGE_LOOP('',(#9221,#9222,#9223,#9224));
#2264=EDGE_LOOP('',(#9225,#9226,#9227,#9228));
#2265=EDGE_LOOP('',(#9229,#9230,#9231,#9232));
#2266=EDGE_LOOP('',(#9233,#9234,#9235,#9236));
#2267=EDGE_LOOP('',(#9237,#9238,#9239,#9240));
#2268=EDGE_LOOP('',(#9241));
#2269=EDGE_LOOP('',(#9242));
#2270=EDGE_LOOP('',(#9243,#9244,#9245,#9246));
#2271=EDGE_LOOP('',(#9247,#9248,#9249,#9250));
#2272=EDGE_LOOP('',(#9251));
#2273=EDGE_LOOP('',(#9252));
#2274=EDGE_LOOP('',(#9253));
#2275=EDGE_LOOP('',(#9254));
#2276=EDGE_LOOP('',(#9255));
#2277=EDGE_LOOP('',(#9256));
#2278=EDGE_LOOP('',(#9257));
#2279=EDGE_LOOP('',(#9258));
#2280=EDGE_LOOP('',(#9259));
#2281=EDGE_LOOP('',(#9260));
#2282=EDGE_LOOP('',(#9261));
#2283=EDGE_LOOP('',(#9262));
#2284=EDGE_LOOP('',(#9263,#9264,#9265,#9266));
#2285=EDGE_LOOP('',(#9267,#9268,#9269,#9270));
#2286=EDGE_LOOP('',(#9271,#9272,#9273,#9274));
#2287=EDGE_LOOP('',(#9275,#9276,#9277,#9278));
#2288=EDGE_LOOP('',(#9279,#9280,#9281,#9282));
#2289=EDGE_LOOP('',(#9283,#9284,#9285,#9286));
#2290=EDGE_LOOP('',(#9287,#9288,#9289,#9290));
#2291=EDGE_LOOP('',(#9291,#9292,#9293,#9294));
#2292=EDGE_LOOP('',(#9295));
#2293=EDGE_LOOP('',(#9296,#9297,#9298,#9299));
#2294=EDGE_LOOP('',(#9300));
#2295=EDGE_LOOP('',(#9301,#9302,#9303,#9304));
#2296=EDGE_LOOP('',(#9305,#9306,#9307,#9308));
#2297=EDGE_LOOP('',(#9309,#9310,#9311,#9312,#9313,#9314,#9315,#9316));
#2298=EDGE_LOOP('',(#9317));
#2299=EDGE_LOOP('',(#9318));
#2300=EDGE_LOOP('',(#9319));
#2301=EDGE_LOOP('',(#9320));
#2302=EDGE_LOOP('',(#9321));
#2303=EDGE_LOOP('',(#9322,#9323,#9324,#9325));
#2304=EDGE_LOOP('',(#9326,#9327,#9328,#9329,#9330,#9331,#9332,#9333));
#2305=EDGE_LOOP('',(#9334));
#2306=EDGE_LOOP('',(#9335));
#2307=EDGE_LOOP('',(#9336));
#2308=EDGE_LOOP('',(#9337));
#2309=EDGE_LOOP('',(#9338));
#2310=EDGE_LOOP('',(#9339,#9340,#9341,#9342));
#2311=EDGE_LOOP('',(#9343,#9344,#9345,#9346));
#2312=EDGE_LOOP('',(#9347,#9348,#9349,#9350));
#2313=EDGE_LOOP('',(#9351));
#2314=EDGE_LOOP('',(#9352));
#2315=EDGE_LOOP('',(#9353,#9354,#9355,#9356));
#2316=EDGE_LOOP('',(#9357,#9358,#9359,#9360));
#2317=EDGE_LOOP('',(#9361,#9362,#9363,#9364));
#2318=EDGE_LOOP('',(#9365,#9366,#9367,#9368));
#2319=EDGE_LOOP('',(#9369,#9370,#9371,#9372));
#2320=EDGE_LOOP('',(#9373));
#2321=EDGE_LOOP('',(#9374));
#2322=EDGE_LOOP('',(#9375,#9376,#9377,#9378));
#2323=EDGE_LOOP('',(#9379,#9380,#9381,#9382));
#2324=EDGE_LOOP('',(#9383));
#2325=EDGE_LOOP('',(#9384));
#2326=EDGE_LOOP('',(#9385));
#2327=EDGE_LOOP('',(#9386));
#2328=EDGE_LOOP('',(#9387));
#2329=EDGE_LOOP('',(#9388));
#2330=EDGE_LOOP('',(#9389));
#2331=EDGE_LOOP('',(#9390));
#2332=EDGE_LOOP('',(#9391));
#2333=EDGE_LOOP('',(#9392));
#2334=EDGE_LOOP('',(#9393));
#2335=EDGE_LOOP('',(#9394));
#2336=EDGE_LOOP('',(#9395,#9396,#9397,#9398));
#2337=EDGE_LOOP('',(#9399,#9400,#9401,#9402));
#2338=EDGE_LOOP('',(#9403,#9404,#9405,#9406));
#2339=EDGE_LOOP('',(#9407,#9408,#9409,#9410));
#2340=EDGE_LOOP('',(#9411,#9412,#9413,#9414));
#2341=EDGE_LOOP('',(#9415));
#2342=EDGE_LOOP('',(#9416));
#2343=EDGE_LOOP('',(#9417,#9418,#9419,#9420));
#2344=EDGE_LOOP('',(#9421,#9422,#9423,#9424));
#2345=EDGE_LOOP('',(#9425));
#2346=EDGE_LOOP('',(#9426));
#2347=EDGE_LOOP('',(#9427));
#2348=EDGE_LOOP('',(#9428));
#2349=EDGE_LOOP('',(#9429));
#2350=EDGE_LOOP('',(#9430));
#2351=EDGE_LOOP('',(#9431));
#2352=EDGE_LOOP('',(#9432));
#2353=EDGE_LOOP('',(#9433));
#2354=EDGE_LOOP('',(#9434));
#2355=EDGE_LOOP('',(#9435));
#2356=EDGE_LOOP('',(#9436));
#2357=EDGE_LOOP('',(#9437));
#2358=EDGE_LOOP('',(#9438,#9439,#9440,#9441));
#2359=EDGE_LOOP('',(#9442,#9443,#9444,#9445));
#2360=EDGE_LOOP('',(#9446));
#2361=EDGE_LOOP('',(#9447,#9448,#9449,#9450,#9451,#9452));
#2362=EDGE_LOOP('',(#9453,#9454,#9455,#9456,#9457));
#2363=EDGE_LOOP('',(#9458,#9459,#9460,#9461));
#2364=EDGE_LOOP('',(#9462,#9463,#9464,#9465));
#2365=EDGE_LOOP('',(#9466));
#2366=EDGE_LOOP('',(#9467));
#2367=EDGE_LOOP('',(#9468,#9469,#9470,#9471,#9472));
#2368=EDGE_LOOP('',(#9473));
#2369=EDGE_LOOP('',(#9474));
#2370=EDGE_LOOP('',(#9475,#9476,#9477,#9478));
#2371=EDGE_LOOP('',(#9479,#9480,#9481,#9482,#9483,#9484));
#2372=EDGE_LOOP('',(#9485,#9486,#9487,#9488,#9489));
#2373=EDGE_LOOP('',(#9490));
#2374=EDGE_LOOP('',(#9491));
#2375=EDGE_LOOP('',(#9492,#9493,#9494,#9495));
#2376=EDGE_LOOP('',(#9496,#9497,#9498,#9499));
#2377=EDGE_LOOP('',(#9500,#9501,#9502,#9503));
#2378=EDGE_LOOP('',(#9504));
#2379=EDGE_LOOP('',(#9505));
#2380=EDGE_LOOP('',(#9506,#9507,#9508,#9509,#9510));
#2381=EDGE_LOOP('',(#9511,#9512));
#2382=EDGE_LOOP('',(#9513,#9514));
#2383=EDGE_LOOP('',(#9515,#9516));
#2384=EDGE_LOOP('',(#9517,#9518));
#2385=EDGE_LOOP('',(#9519,#9520));
#2386=EDGE_LOOP('',(#9521,#9522));
#2387=EDGE_LOOP('',(#9523,#9524));
#2388=EDGE_LOOP('',(#9525,#9526,#9527,#9528));
#2389=EDGE_LOOP('',(#9529,#9530,#9531,#9532,#9533,#9534,#9535,#9536,#9537,
#9538,#9539,#9540,#9541,#9542,#9543,#9544,#9545,#9546));
#2390=EDGE_LOOP('',(#9547,#9548,#9549,#9550));
#2391=EDGE_LOOP('',(#9551,#9552,#9553,#9554));
#2392=EDGE_LOOP('',(#9555,#9556,#9557,#9558));
#2393=EDGE_LOOP('',(#9559,#9560,#9561,#9562));
#2394=EDGE_LOOP('',(#9563,#9564,#9565,#9566,#9567,#9568));
#2395=EDGE_LOOP('',(#9569,#9570,#9571,#9572));
#2396=EDGE_LOOP('',(#9573,#9574,#9575,#9576));
#2397=EDGE_LOOP('',(#9577,#9578,#9579,#9580));
#2398=EDGE_LOOP('',(#9581,#9582,#9583,#9584));
#2399=EDGE_LOOP('',(#9585,#9586,#9587,#9588));
#2400=EDGE_LOOP('',(#9589,#9590,#9591,#9592,#9593,#9594,#9595,#9596,#9597,
#9598,#9599,#9600,#9601,#9602,#9603,#9604,#9605,#9606));
#2401=EDGE_LOOP('',(#9607,#9608,#9609,#9610));
#2402=EDGE_LOOP('',(#9611,#9612,#9613,#9614));
#2403=EDGE_LOOP('',(#9615));
#2404=EDGE_LOOP('',(#9616));
#2405=EDGE_LOOP('',(#9617,#9618,#9619,#9620));
#2406=EDGE_LOOP('',(#9621));
#2407=EDGE_LOOP('',(#9622));
#2408=EDGE_LOOP('',(#9623,#9624,#9625,#9626));
#2409=EDGE_LOOP('',(#9627));
#2410=EDGE_LOOP('',(#9628));
#2411=EDGE_LOOP('',(#9629,#9630,#9631,#9632));
#2412=EDGE_LOOP('',(#9633));
#2413=EDGE_LOOP('',(#9634));
#2414=EDGE_LOOP('',(#9635,#9636,#9637,#9638));
#2415=EDGE_LOOP('',(#9639));
#2416=EDGE_LOOP('',(#9640));
#2417=EDGE_LOOP('',(#9641,#9642,#9643,#9644));
#2418=EDGE_LOOP('',(#9645,#9646,#9647,#9648));
#2419=EDGE_LOOP('',(#9649,#9650,#9651,#9652));
#2420=EDGE_LOOP('',(#9653,#9654,#9655,#9656));
#2421=EDGE_LOOP('',(#9657,#9658,#9659,#9660));
#2422=EDGE_LOOP('',(#9661,#9662,#9663,#9664));
#2423=EDGE_LOOP('',(#9665,#9666,#9667,#9668));
#2424=EDGE_LOOP('',(#9669,#9670,#9671,#9672,#9673,#9674));
#2425=EDGE_LOOP('',(#9675,#9676,#9677,#9678,#9679,#9680));
#2426=EDGE_LOOP('',(#9681));
#2427=EDGE_LOOP('',(#9682));
#2428=EDGE_LOOP('',(#9683,#9684,#9685,#9686));
#2429=EDGE_LOOP('',(#9687,#9688,#9689,#9690));
#2430=EDGE_LOOP('',(#9691,#9692,#9693,#9694));
#2431=EDGE_LOOP('',(#9695));
#2432=EDGE_LOOP('',(#9696));
#2433=EDGE_LOOP('',(#9697,#9698,#9699,#9700));
#2434=EDGE_LOOP('',(#9701,#9702,#9703,#9704));
#2435=EDGE_LOOP('',(#9705,#9706,#9707,#9708));
#2436=EDGE_LOOP('',(#9709));
#2437=EDGE_LOOP('',(#9710,#9711,#9712,#9713));
#2438=EDGE_LOOP('',(#9714,#9715,#9716,#9717));
#2439=EDGE_LOOP('',(#9718,#9719,#9720,#9721,#9722,#9723,#9724));
#2440=EDGE_LOOP('',(#9725,#9726,#9727,#9728,#9729,#9730,#9731));
#2441=EDGE_LOOP('',(#9732,#9733,#9734,#9735));
#2442=EDGE_LOOP('',(#9736,#9737,#9738,#9739));
#2443=EDGE_LOOP('',(#9740,#9741,#9742,#9743));
#2444=EDGE_LOOP('',(#9744,#9745,#9746,#9747));
#2445=EDGE_LOOP('',(#9748,#9749,#9750,#9751));
#2446=EDGE_LOOP('',(#9752,#9753,#9754,#9755));
#2447=EDGE_LOOP('',(#9756,#9757,#9758,#9759));
#2448=EDGE_LOOP('',(#9760,#9761,#9762,#9763));
#2449=EDGE_LOOP('',(#9764,#9765,#9766,#9767));
#2450=EDGE_LOOP('',(#9768,#9769,#9770,#9771));
#2451=EDGE_LOOP('',(#9772,#9773,#9774,#9775));
#2452=EDGE_LOOP('',(#9776,#9777,#9778,#9779));
#2453=EDGE_LOOP('',(#9780,#9781,#9782,#9783));
#2454=EDGE_LOOP('',(#9784,#9785,#9786,#9787));
#2455=EDGE_LOOP('',(#9788,#9789,#9790,#9791));
#2456=EDGE_LOOP('',(#9792,#9793,#9794,#9795));
#2457=EDGE_LOOP('',(#9796,#9797,#9798,#9799));
#2458=EDGE_LOOP('',(#9800,#9801,#9802,#9803));
#2459=EDGE_LOOP('',(#9804,#9805,#9806,#9807));
#2460=EDGE_LOOP('',(#9808,#9809,#9810,#9811));
#2461=EDGE_LOOP('',(#9812,#9813,#9814,#9815));
#2462=EDGE_LOOP('',(#9816,#9817,#9818,#9819));
#2463=EDGE_LOOP('',(#9820,#9821,#9822,#9823));
#2464=EDGE_LOOP('',(#9824,#9825,#9826,#9827));
#2465=EDGE_LOOP('',(#9828,#9829,#9830,#9831));
#2466=EDGE_LOOP('',(#9832,#9833,#9834,#9835));
#2467=EDGE_LOOP('',(#9836,#9837,#9838,#9839));
#2468=EDGE_LOOP('',(#9840,#9841,#9842,#9843));
#2469=EDGE_LOOP('',(#9844,#9845,#9846,#9847));
#2470=EDGE_LOOP('',(#9848,#9849,#9850,#9851));
#2471=EDGE_LOOP('',(#9852,#9853,#9854,#9855));
#2472=EDGE_LOOP('',(#9856,#9857,#9858,#9859));
#2473=EDGE_LOOP('',(#9860,#9861,#9862,#9863));
#2474=EDGE_LOOP('',(#9864,#9865,#9866,#9867));
#2475=EDGE_LOOP('',(#9868,#9869,#9870,#9871));
#2476=EDGE_LOOP('',(#9872,#9873,#9874,#9875));
#2477=EDGE_LOOP('',(#9876,#9877,#9878,#9879));
#2478=EDGE_LOOP('',(#9880,#9881,#9882,#9883));
#2479=EDGE_LOOP('',(#9884,#9885,#9886,#9887));
#2480=EDGE_LOOP('',(#9888,#9889,#9890,#9891));
#2481=EDGE_LOOP('',(#9892,#9893,#9894,#9895));
#2482=EDGE_LOOP('',(#9896,#9897,#9898,#9899));
#2483=EDGE_LOOP('',(#9900,#9901,#9902,#9903));
#2484=EDGE_LOOP('',(#9904,#9905,#9906,#9907));
#2485=EDGE_LOOP('',(#9908,#9909,#9910,#9911));
#2486=EDGE_LOOP('',(#9912,#9913,#9914,#9915));
#2487=EDGE_LOOP('',(#9916,#9917,#9918,#9919));
#2488=EDGE_LOOP('',(#9920,#9921,#9922,#9923));
#2489=EDGE_LOOP('',(#9924,#9925,#9926,#9927));
#2490=EDGE_LOOP('',(#9928,#9929,#9930,#9931));
#2491=EDGE_LOOP('',(#9932,#9933,#9934,#9935));
#2492=EDGE_LOOP('',(#9936,#9937,#9938,#9939));
#2493=EDGE_LOOP('',(#9940,#9941,#9942,#9943));
#2494=EDGE_LOOP('',(#9944,#9945,#9946,#9947));
#2495=EDGE_LOOP('',(#9948,#9949,#9950,#9951));
#2496=EDGE_LOOP('',(#9952,#9953,#9954,#9955));
#2497=EDGE_LOOP('',(#9956,#9957,#9958,#9959));
#2498=EDGE_LOOP('',(#9960,#9961,#9962,#9963));
#2499=EDGE_LOOP('',(#9964,#9965,#9966,#9967));
#2500=EDGE_LOOP('',(#9968,#9969,#9970,#9971));
#2501=EDGE_LOOP('',(#9972,#9973,#9974,#9975));
#2502=EDGE_LOOP('',(#9976,#9977,#9978,#9979));
#2503=EDGE_LOOP('',(#9980,#9981,#9982,#9983));
#2504=EDGE_LOOP('',(#9984,#9985,#9986,#9987));
#2505=EDGE_LOOP('',(#9988,#9989,#9990,#9991));
#2506=EDGE_LOOP('',(#9992,#9993,#9994,#9995));
#2507=EDGE_LOOP('',(#9996,#9997,#9998,#9999));
#2508=EDGE_LOOP('',(#10000,#10001,#10002,#10003));
#2509=EDGE_LOOP('',(#10004,#10005,#10006,#10007));
#2510=EDGE_LOOP('',(#10008,#10009,#10010,#10011));
#2511=EDGE_LOOP('',(#10012,#10013,#10014,#10015));
#2512=EDGE_LOOP('',(#10016,#10017,#10018,#10019));
#2513=EDGE_LOOP('',(#10020,#10021,#10022,#10023));
#2514=EDGE_LOOP('',(#10024,#10025,#10026,#10027));
#2515=EDGE_LOOP('',(#10028,#10029,#10030,#10031));
#2516=EDGE_LOOP('',(#10032,#10033,#10034,#10035));
#2517=EDGE_LOOP('',(#10036,#10037,#10038,#10039));
#2518=EDGE_LOOP('',(#10040,#10041,#10042,#10043));
#2519=EDGE_LOOP('',(#10044,#10045,#10046,#10047));
#2520=EDGE_LOOP('',(#10048,#10049,#10050,#10051));
#2521=EDGE_LOOP('',(#10052,#10053,#10054,#10055));
#2522=EDGE_LOOP('',(#10056,#10057,#10058,#10059));
#2523=EDGE_LOOP('',(#10060,#10061,#10062,#10063));
#2524=EDGE_LOOP('',(#10064,#10065,#10066,#10067));
#2525=EDGE_LOOP('',(#10068,#10069,#10070,#10071));
#2526=EDGE_LOOP('',(#10072,#10073,#10074,#10075));
#2527=EDGE_LOOP('',(#10076,#10077,#10078,#10079));
#2528=EDGE_LOOP('',(#10080,#10081,#10082,#10083));
#2529=EDGE_LOOP('',(#10084,#10085,#10086,#10087));
#2530=EDGE_LOOP('',(#10088,#10089,#10090,#10091));
#2531=EDGE_LOOP('',(#10092,#10093,#10094,#10095));
#2532=EDGE_LOOP('',(#10096,#10097,#10098,#10099));
#2533=EDGE_LOOP('',(#10100,#10101,#10102,#10103));
#2534=EDGE_LOOP('',(#10104,#10105,#10106,#10107));
#2535=EDGE_LOOP('',(#10108,#10109,#10110,#10111));
#2536=EDGE_LOOP('',(#10112,#10113,#10114,#10115));
#2537=EDGE_LOOP('',(#10116,#10117,#10118,#10119));
#2538=EDGE_LOOP('',(#10120,#10121,#10122,#10123));
#2539=EDGE_LOOP('',(#10124,#10125,#10126,#10127));
#2540=EDGE_LOOP('',(#10128,#10129,#10130,#10131));
#2541=EDGE_LOOP('',(#10132,#10133,#10134,#10135));
#2542=EDGE_LOOP('',(#10136,#10137,#10138,#10139));
#2543=EDGE_LOOP('',(#10140,#10141,#10142,#10143));
#2544=EDGE_LOOP('',(#10144,#10145,#10146,#10147));
#2545=EDGE_LOOP('',(#10148,#10149,#10150,#10151));
#2546=EDGE_LOOP('',(#10152,#10153,#10154,#10155));
#2547=EDGE_LOOP('',(#10156,#10157,#10158,#10159));
#2548=EDGE_LOOP('',(#10160,#10161,#10162,#10163));
#2549=EDGE_LOOP('',(#10164,#10165,#10166,#10167));
#2550=EDGE_LOOP('',(#10168,#10169,#10170,#10171));
#2551=EDGE_LOOP('',(#10172,#10173,#10174,#10175));
#2552=EDGE_LOOP('',(#10176,#10177,#10178,#10179));
#2553=EDGE_LOOP('',(#10180,#10181,#10182,#10183));
#2554=EDGE_LOOP('',(#10184,#10185,#10186,#10187));
#2555=EDGE_LOOP('',(#10188,#10189,#10190,#10191));
#2556=EDGE_LOOP('',(#10192,#10193,#10194,#10195));
#2557=EDGE_LOOP('',(#10196,#10197,#10198,#10199));
#2558=EDGE_LOOP('',(#10200,#10201,#10202,#10203));
#2559=EDGE_LOOP('',(#10204,#10205,#10206,#10207));
#2560=EDGE_LOOP('',(#10208,#10209,#10210,#10211));
#2561=EDGE_LOOP('',(#10212,#10213,#10214,#10215));
#2562=EDGE_LOOP('',(#10216,#10217,#10218,#10219));
#2563=EDGE_LOOP('',(#10220,#10221,#10222,#10223));
#2564=EDGE_LOOP('',(#10224,#10225,#10226,#10227));
#2565=EDGE_LOOP('',(#10228,#10229,#10230,#10231));
#2566=EDGE_LOOP('',(#10232,#10233,#10234,#10235));
#2567=EDGE_LOOP('',(#10236,#10237,#10238,#10239));
#2568=EDGE_LOOP('',(#10240,#10241,#10242,#10243));
#2569=EDGE_LOOP('',(#10244,#10245,#10246,#10247));
#2570=EDGE_LOOP('',(#10248,#10249,#10250,#10251));
#2571=EDGE_LOOP('',(#10252,#10253,#10254,#10255));
#2572=EDGE_LOOP('',(#10256,#10257,#10258,#10259));
#2573=EDGE_LOOP('',(#10260,#10261,#10262,#10263));
#2574=EDGE_LOOP('',(#10264,#10265,#10266,#10267));
#2575=EDGE_LOOP('',(#10268,#10269,#10270,#10271));
#2576=EDGE_LOOP('',(#10272,#10273,#10274,#10275));
#2577=EDGE_LOOP('',(#10276,#10277,#10278,#10279));
#2578=EDGE_LOOP('',(#10280,#10281,#10282,#10283));
#2579=EDGE_LOOP('',(#10284,#10285,#10286,#10287));
#2580=EDGE_LOOP('',(#10288,#10289,#10290,#10291));
#2581=EDGE_LOOP('',(#10292,#10293,#10294,#10295));
#2582=EDGE_LOOP('',(#10296,#10297,#10298,#10299));
#2583=EDGE_LOOP('',(#10300,#10301,#10302,#10303));
#2584=EDGE_LOOP('',(#10304,#10305,#10306,#10307));
#2585=EDGE_LOOP('',(#10308,#10309,#10310,#10311));
#2586=EDGE_LOOP('',(#10312,#10313,#10314,#10315));
#2587=EDGE_LOOP('',(#10316,#10317,#10318,#10319));
#2588=EDGE_LOOP('',(#10320,#10321,#10322,#10323));
#2589=EDGE_LOOP('',(#10324,#10325,#10326,#10327));
#2590=EDGE_LOOP('',(#10328,#10329,#10330,#10331));
#2591=EDGE_LOOP('',(#10332,#10333,#10334,#10335));
#2592=EDGE_LOOP('',(#10336,#10337,#10338,#10339));
#2593=EDGE_LOOP('',(#10340,#10341,#10342,#10343));
#2594=EDGE_LOOP('',(#10344,#10345,#10346,#10347));
#2595=EDGE_LOOP('',(#10348,#10349,#10350,#10351));
#2596=EDGE_LOOP('',(#10352,#10353,#10354,#10355));
#2597=EDGE_LOOP('',(#10356,#10357,#10358,#10359));
#2598=EDGE_LOOP('',(#10360,#10361,#10362,#10363));
#2599=EDGE_LOOP('',(#10364,#10365,#10366,#10367));
#2600=EDGE_LOOP('',(#10368,#10369,#10370,#10371));
#2601=EDGE_LOOP('',(#10372,#10373,#10374,#10375));
#2602=EDGE_LOOP('',(#10376,#10377,#10378,#10379,#10380,#10381,#10382,#10383,
#10384,#10385,#10386,#10387,#10388,#10389,#10390,#10391,#10392,#10393,#10394,
#10395,#10396,#10397,#10398,#10399,#10400,#10401,#10402,#10403,#10404,#10405,
#10406,#10407,#10408,#10409,#10410,#10411,#10412,#10413,#10414,#10415,#10416,
#10417,#10418,#10419,#10420,#10421,#10422,#10423,#10424,#10425,#10426,#10427,
#10428,#10429,#10430,#10431,#10432,#10433,#10434,#10435,#10436,#10437,#10438,
#10439,#10440,#10441,#10442,#10443,#10444,#10445,#10446,#10447,#10448,#10449,
#10450,#10451,#10452,#10453,#10454,#10455,#10456,#10457,#10458,#10459,#10460,
#10461,#10462,#10463,#10464,#10465,#10466,#10467,#10468,#10469,#10470,#10471,
#10472,#10473,#10474,#10475,#10476,#10477,#10478,#10479,#10480,#10481,#10482,
#10483,#10484,#10485,#10486,#10487,#10488,#10489,#10490,#10491,#10492,#10493,
#10494,#10495,#10496,#10497,#10498,#10499,#10500,#10501,#10502,#10503,#10504,
#10505,#10506,#10507,#10508,#10509,#10510,#10511,#10512,#10513,#10514,#10515,
#10516,#10517,#10518,#10519,#10520,#10521,#10522,#10523,#10524,#10525,#10526,
#10527,#10528,#10529,#10530,#10531,#10532,#10533,#10534,#10535,#10536,#10537,
#10538,#10539));
#2603=EDGE_LOOP('',(#10540,#10541,#10542,#10543,#10544,#10545,#10546,#10547,
#10548,#10549,#10550,#10551,#10552,#10553,#10554,#10555,#10556,#10557,#10558,
#10559,#10560,#10561,#10562,#10563,#10564,#10565,#10566,#10567,#10568,#10569,
#10570,#10571,#10572,#10573,#10574,#10575,#10576,#10577,#10578,#10579,#10580,
#10581,#10582,#10583,#10584,#10585,#10586,#10587,#10588,#10589,#10590,#10591,
#10592,#10593,#10594,#10595,#10596,#10597,#10598,#10599,#10600,#10601,#10602,
#10603,#10604,#10605,#10606,#10607,#10608,#10609,#10610,#10611,#10612,#10613,
#10614,#10615,#10616,#10617,#10618,#10619,#10620,#10621,#10622,#10623,#10624,
#10625,#10626,#10627,#10628,#10629,#10630,#10631,#10632,#10633,#10634,#10635,
#10636,#10637,#10638,#10639,#10640,#10641,#10642,#10643,#10644,#10645,#10646,
#10647,#10648,#10649,#10650,#10651,#10652,#10653,#10654,#10655,#10656,#10657,
#10658,#10659,#10660,#10661,#10662,#10663,#10664,#10665,#10666,#10667,#10668,
#10669,#10670,#10671,#10672,#10673,#10674,#10675,#10676,#10677,#10678,#10679,
#10680,#10681,#10682,#10683,#10684,#10685,#10686,#10687,#10688,#10689,#10690,
#10691,#10692,#10693,#10694,#10695,#10696,#10697,#10698,#10699,#10700,#10701,
#10702,#10703));
#2604=EDGE_LOOP('',(#10704,#10705,#10706,#10707,#10708,#10709,#10710,#10711,
#10712,#10713,#10714,#10715));
#2605=EDGE_LOOP('',(#10716));
#2606=EDGE_LOOP('',(#10717));
#2607=EDGE_LOOP('',(#10718));
#2608=EDGE_LOOP('',(#10719,#10720));
#2609=EDGE_LOOP('',(#10721,#10722,#10723,#10724,#10725,#10726,#10727,#10728,
#10729));
#2610=EDGE_LOOP('',(#10730,#10731));
#2611=EDGE_LOOP('',(#10732,#10733,#10734,#10735));
#2612=EDGE_LOOP('',(#10736,#10737,#10738,#10739,#10740));
#2613=EDGE_LOOP('',(#10741,#10742,#10743,#10744));
#2614=EDGE_LOOP('',(#10745));
#2615=EDGE_LOOP('',(#10746));
#2616=EDGE_LOOP('',(#10747,#10748,#10749,#10750));
#2617=EDGE_LOOP('',(#10751,#10752));
#2618=EDGE_LOOP('',(#10753));
#2619=EDGE_LOOP('',(#10754));
#2620=EDGE_LOOP('',(#10755));
#2621=EDGE_LOOP('',(#10756));
#2622=EDGE_LOOP('',(#10757,#10758,#10759,#10760));
#2623=EDGE_LOOP('',(#10761));
#2624=EDGE_LOOP('',(#10762));
#2625=EDGE_LOOP('',(#10763,#10764,#10765,#10766));
#2626=EDGE_LOOP('',(#10767));
#2627=EDGE_LOOP('',(#10768));
#2628=EDGE_LOOP('',(#10769,#10770,#10771,#10772,#10773,#10774));
#2629=EDGE_LOOP('',(#10775,#10776,#10777,#10778));
#2630=EDGE_LOOP('',(#10779,#10780,#10781,#10782));
#2631=EDGE_LOOP('',(#10783,#10784,#10785,#10786));
#2632=EDGE_LOOP('',(#10787,#10788,#10789,#10790));
#2633=EDGE_LOOP('',(#10791,#10792,#10793,#10794,#10795,#10796));
#2634=EDGE_LOOP('',(#10797,#10798,#10799,#10800));
#2635=EDGE_LOOP('',(#10801,#10802));
#2636=EDGE_LOOP('',(#10803,#10804,#10805,#10806));
#2637=EDGE_LOOP('',(#10807,#10808));
#2638=EDGE_LOOP('',(#10809,#10810,#10811,#10812,#10813,#10814));
#2639=EDGE_LOOP('',(#10815,#10816,#10817,#10818));
#2640=EDGE_LOOP('',(#10819,#10820,#10821,#10822));
#2641=EDGE_LOOP('',(#10823,#10824,#10825,#10826));
#2642=EDGE_LOOP('',(#10827,#10828,#10829,#10830));
#2643=EDGE_LOOP('',(#10831,#10832,#10833,#10834));
#2644=EDGE_LOOP('',(#10835,#10836,#10837,#10838));
#2645=EDGE_LOOP('',(#10839,#10840,#10841,#10842,#10843,#10844));
#2646=EDGE_LOOP('',(#10845));
#2647=EDGE_LOOP('',(#10846,#10847,#10848,#10849,#10850,#10851));
#2648=EDGE_LOOP('',(#10852,#10853,#10854,#10855));
#2649=EDGE_LOOP('',(#10856,#10857,#10858,#10859));
#2650=EDGE_LOOP('',(#10860,#10861,#10862,#10863));
#2651=EDGE_LOOP('',(#10864));
#2652=EDGE_LOOP('',(#10865,#10866,#10867,#10868));
#2653=EDGE_LOOP('',(#10869));
#2654=EDGE_LOOP('',(#10870,#10871,#10872,#10873));
#2655=EDGE_LOOP('',(#10874));
#2656=EDGE_LOOP('',(#10875,#10876,#10877,#10878));
#2657=EDGE_LOOP('',(#10879,#10880,#10881,#10882));
#2658=EDGE_LOOP('',(#10883,#10884,#10885,#10886));
#2659=EDGE_LOOP('',(#10887,#10888,#10889,#10890));
#2660=EDGE_LOOP('',(#10891,#10892,#10893,#10894));
#2661=EDGE_LOOP('',(#10895,#10896,#10897,#10898));
#2662=EDGE_LOOP('',(#10899,#10900,#10901,#10902));
#2663=EDGE_LOOP('',(#10903,#10904,#10905,#10906));
#2664=EDGE_LOOP('',(#10907,#10908,#10909,#10910));
#2665=EDGE_LOOP('',(#10911,#10912,#10913,#10914));
#2666=EDGE_LOOP('',(#10915,#10916,#10917,#10918));
#2667=EDGE_LOOP('',(#10919,#10920,#10921,#10922));
#2668=EDGE_LOOP('',(#10923,#10924,#10925,#10926));
#2669=EDGE_LOOP('',(#10927));
#2670=EDGE_LOOP('',(#10928));
#2671=EDGE_LOOP('',(#10929));
#2672=EDGE_LOOP('',(#10930));
#2673=EDGE_LOOP('',(#10931,#10932,#10933,#10934));
#2674=EDGE_LOOP('',(#10935,#10936,#10937,#10938));
#2675=EDGE_LOOP('',(#10939));
#2676=EDGE_LOOP('',(#10940));
#2677=EDGE_LOOP('',(#10941));
#2678=EDGE_LOOP('',(#10942));
#2679=EDGE_LOOP('',(#10943,#10944,#10945,#10946));
#2680=EDGE_LOOP('',(#10947,#10948,#10949,#10950));
#2681=EDGE_LOOP('',(#10951));
#2682=EDGE_LOOP('',(#10952));
#2683=EDGE_LOOP('',(#10953));
#2684=EDGE_LOOP('',(#10954));
#2685=EDGE_LOOP('',(#10955,#10956,#10957,#10958));
#2686=EDGE_LOOP('',(#10959,#10960,#10961,#10962));
#2687=EDGE_LOOP('',(#10963));
#2688=EDGE_LOOP('',(#10964));
#2689=EDGE_LOOP('',(#10965));
#2690=EDGE_LOOP('',(#10966));
#2691=EDGE_LOOP('',(#10967,#10968,#10969,#10970));
#2692=EDGE_LOOP('',(#10971,#10972,#10973,#10974));
#2693=EDGE_LOOP('',(#10975));
#2694=EDGE_LOOP('',(#10976));
#2695=EDGE_LOOP('',(#10977));
#2696=EDGE_LOOP('',(#10978));
#2697=EDGE_LOOP('',(#10979,#10980,#10981,#10982));
#2698=EDGE_LOOP('',(#10983,#10984,#10985,#10986));
#2699=EDGE_LOOP('',(#10987,#10988,#10989,#10990));
#2700=EDGE_LOOP('',(#10991,#10992,#10993,#10994));
#2701=EDGE_LOOP('',(#10995,#10996,#10997,#10998));
#2702=EDGE_LOOP('',(#10999,#11000,#11001,#11002));
#2703=EDGE_LOOP('',(#11003,#11004,#11005,#11006));
#2704=EDGE_LOOP('',(#11007,#11008,#11009,#11010));
#2705=EDGE_LOOP('',(#11011,#11012,#11013,#11014));
#2706=EDGE_LOOP('',(#11015,#11016,#11017,#11018));
#2707=EDGE_LOOP('',(#11019,#11020,#11021,#11022));
#2708=EDGE_LOOP('',(#11023,#11024,#11025,#11026));
#2709=EDGE_LOOP('',(#11027,#11028,#11029,#11030));
#2710=EDGE_LOOP('',(#11031,#11032,#11033,#11034));
#2711=EDGE_LOOP('',(#11035,#11036,#11037,#11038));
#2712=EDGE_LOOP('',(#11039,#11040,#11041,#11042));
#2713=EDGE_LOOP('',(#11043));
#2714=EDGE_LOOP('',(#11044,#11045,#11046,#11047));
#2715=EDGE_LOOP('',(#11048,#11049,#11050,#11051));
#2716=EDGE_LOOP('',(#11052,#11053,#11054,#11055));
#2717=EDGE_LOOP('',(#11056,#11057,#11058,#11059));
#2718=EDGE_LOOP('',(#11060,#11061,#11062,#11063));
#2719=EDGE_LOOP('',(#11064));
#2720=EDGE_LOOP('',(#11065,#11066,#11067,#11068));
#2721=EDGE_LOOP('',(#11069,#11070,#11071,#11072));
#2722=EDGE_LOOP('',(#11073));
#2723=EDGE_LOOP('',(#11074,#11075,#11076,#11077));
#2724=EDGE_LOOP('',(#11078,#11079,#11080,#11081));
#2725=EDGE_LOOP('',(#11082));
#2726=EDGE_LOOP('',(#11083,#11084,#11085,#11086));
#2727=EDGE_LOOP('',(#11087,#11088,#11089,#11090));
#2728=EDGE_LOOP('',(#11091,#11092,#11093,#11094));
#2729=EDGE_LOOP('',(#11095));
#2730=EDGE_LOOP('',(#11096));
#2731=EDGE_LOOP('',(#11097));
#2732=EDGE_LOOP('',(#11098));
#2733=EDGE_LOOP('',(#11099,#11100,#11101,#11102));
#2734=EDGE_LOOP('',(#11103,#11104,#11105,#11106));
#2735=EDGE_LOOP('',(#11107));
#2736=EDGE_LOOP('',(#11108));
#2737=EDGE_LOOP('',(#11109));
#2738=EDGE_LOOP('',(#11110));
#2739=EDGE_LOOP('',(#11111,#11112,#11113,#11114));
#2740=EDGE_LOOP('',(#11115,#11116,#11117,#11118));
#2741=EDGE_LOOP('',(#11119));
#2742=EDGE_LOOP('',(#11120));
#2743=EDGE_LOOP('',(#11121));
#2744=EDGE_LOOP('',(#11122));
#2745=EDGE_LOOP('',(#11123,#11124,#11125,#11126));
#2746=EDGE_LOOP('',(#11127,#11128,#11129,#11130));
#2747=EDGE_LOOP('',(#11131,#11132,#11133,#11134));
#2748=EDGE_LOOP('',(#11135,#11136,#11137,#11138,#11139,#11140,#11141,#11142,
#11143,#11144,#11145,#11146,#11147,#11148,#11149,#11150,#11151,#11152,#11153,
#11154,#11155,#11156,#11157,#11158,#11159,#11160,#11161,#11162,#11163,#11164,
#11165,#11166,#11167,#11168,#11169,#11170,#11171,#11172,#11173,#11174,#11175,
#11176,#11177,#11178,#11179,#11180,#11181,#11182,#11183,#11184,#11185,#11186,
#11187,#11188,#11189,#11190,#11191,#11192,#11193,#11194,#11195,#11196,#11197,
#11198,#11199,#11200,#11201,#11202,#11203,#11204,#11205,#11206,#11207,#11208,
#11209,#11210,#11211,#11212,#11213,#11214));
#2749=EDGE_LOOP('',(#11215,#11216,#11217,#11218));
#2750=EDGE_LOOP('',(#11219,#11220,#11221,#11222));
#2751=EDGE_LOOP('',(#11223,#11224,#11225,#11226));
#2752=EDGE_LOOP('',(#11227));
#2753=EDGE_LOOP('',(#11228,#11229,#11230,#11231));
#2754=EDGE_LOOP('',(#11232,#11233,#11234,#11235));
#2755=EDGE_LOOP('',(#11236,#11237,#11238,#11239));
#2756=EDGE_LOOP('',(#11240,#11241,#11242,#11243));
#2757=EDGE_LOOP('',(#11244,#11245,#11246,#11247));
#2758=EDGE_LOOP('',(#11248,#11249,#11250,#11251));
#2759=EDGE_LOOP('',(#11252,#11253,#11254,#11255));
#2760=EDGE_LOOP('',(#11256,#11257,#11258,#11259));
#2761=EDGE_LOOP('',(#11260,#11261,#11262,#11263));
#2762=EDGE_LOOP('',(#11264,#11265,#11266,#11267));
#2763=EDGE_LOOP('',(#11268,#11269,#11270,#11271));
#2764=EDGE_LOOP('',(#11272,#11273,#11274,#11275));
#2765=EDGE_LOOP('',(#11276,#11277,#11278,#11279));
#2766=EDGE_LOOP('',(#11280,#11281,#11282,#11283));
#2767=EDGE_LOOP('',(#11284,#11285,#11286,#11287));
#2768=EDGE_LOOP('',(#11288,#11289,#11290,#11291));
#2769=EDGE_LOOP('',(#11292,#11293,#11294,#11295));
#2770=EDGE_LOOP('',(#11296,#11297,#11298,#11299));
#2771=EDGE_LOOP('',(#11300,#11301,#11302,#11303));
#2772=EDGE_LOOP('',(#11304,#11305,#11306,#11307));
#2773=EDGE_LOOP('',(#11308,#11309,#11310,#11311));
#2774=EDGE_LOOP('',(#11312,#11313,#11314,#11315));
#2775=EDGE_LOOP('',(#11316,#11317,#11318,#11319));
#2776=EDGE_LOOP('',(#11320,#11321,#11322,#11323));
#2777=EDGE_LOOP('',(#11324,#11325,#11326,#11327));
#2778=EDGE_LOOP('',(#11328,#11329,#11330,#11331));
#2779=EDGE_LOOP('',(#11332,#11333,#11334,#11335));
#2780=EDGE_LOOP('',(#11336,#11337,#11338,#11339));
#2781=EDGE_LOOP('',(#11340,#11341,#11342,#11343));
#2782=EDGE_LOOP('',(#11344,#11345,#11346,#11347));
#2783=EDGE_LOOP('',(#11348,#11349,#11350,#11351));
#2784=EDGE_LOOP('',(#11352,#11353,#11354,#11355));
#2785=EDGE_LOOP('',(#11356,#11357,#11358,#11359));
#2786=EDGE_LOOP('',(#11360,#11361,#11362,#11363));
#2787=EDGE_LOOP('',(#11364,#11365,#11366,#11367));
#2788=EDGE_LOOP('',(#11368,#11369,#11370,#11371));
#2789=EDGE_LOOP('',(#11372,#11373,#11374,#11375));
#2790=EDGE_LOOP('',(#11376,#11377,#11378,#11379));
#2791=EDGE_LOOP('',(#11380,#11381,#11382,#11383));
#2792=EDGE_LOOP('',(#11384,#11385,#11386,#11387));
#2793=EDGE_LOOP('',(#11388,#11389,#11390,#11391));
#2794=EDGE_LOOP('',(#11392,#11393,#11394,#11395));
#2795=EDGE_LOOP('',(#11396,#11397,#11398,#11399));
#2796=EDGE_LOOP('',(#11400,#11401,#11402,#11403));
#2797=EDGE_LOOP('',(#11404,#11405,#11406,#11407));
#2798=EDGE_LOOP('',(#11408,#11409,#11410,#11411));
#2799=EDGE_LOOP('',(#11412,#11413,#11414,#11415));
#2800=EDGE_LOOP('',(#11416,#11417,#11418,#11419));
#2801=EDGE_LOOP('',(#11420,#11421,#11422,#11423));
#2802=EDGE_LOOP('',(#11424,#11425,#11426,#11427));
#2803=EDGE_LOOP('',(#11428,#11429,#11430,#11431));
#2804=EDGE_LOOP('',(#11432,#11433,#11434,#11435));
#2805=EDGE_LOOP('',(#11436,#11437,#11438,#11439));
#2806=EDGE_LOOP('',(#11440,#11441,#11442,#11443));
#2807=EDGE_LOOP('',(#11444,#11445,#11446,#11447));
#2808=EDGE_LOOP('',(#11448,#11449,#11450,#11451));
#2809=EDGE_LOOP('',(#11452,#11453,#11454,#11455));
#2810=EDGE_LOOP('',(#11456,#11457,#11458,#11459));
#2811=EDGE_LOOP('',(#11460,#11461,#11462,#11463));
#2812=EDGE_LOOP('',(#11464,#11465,#11466,#11467));
#2813=EDGE_LOOP('',(#11468,#11469,#11470,#11471));
#2814=EDGE_LOOP('',(#11472,#11473,#11474,#11475));
#2815=EDGE_LOOP('',(#11476,#11477,#11478,#11479));
#2816=EDGE_LOOP('',(#11480,#11481,#11482,#11483));
#2817=EDGE_LOOP('',(#11484,#11485,#11486,#11487));
#2818=EDGE_LOOP('',(#11488,#11489,#11490,#11491));
#2819=EDGE_LOOP('',(#11492,#11493,#11494,#11495));
#2820=EDGE_LOOP('',(#11496,#11497,#11498,#11499));
#2821=EDGE_LOOP('',(#11500,#11501,#11502,#11503));
#2822=EDGE_LOOP('',(#11504,#11505,#11506,#11507));
#2823=EDGE_LOOP('',(#11508,#11509,#11510,#11511));
#2824=EDGE_LOOP('',(#11512,#11513,#11514,#11515));
#2825=EDGE_LOOP('',(#11516,#11517,#11518,#11519));
#2826=EDGE_LOOP('',(#11520,#11521,#11522,#11523));
#2827=EDGE_LOOP('',(#11524,#11525,#11526,#11527));
#2828=EDGE_LOOP('',(#11528,#11529,#11530,#11531));
#2829=EDGE_LOOP('',(#11532,#11533,#11534,#11535));
#2830=EDGE_LOOP('',(#11536,#11537,#11538,#11539));
#2831=EDGE_LOOP('',(#11540,#11541,#11542,#11543));
#2832=EDGE_LOOP('',(#11544,#11545,#11546,#11547));
#2833=EDGE_LOOP('',(#11548,#11549,#11550,#11551,#11552,#11553,#11554,#11555,
#11556,#11557,#11558,#11559,#11560,#11561,#11562,#11563,#11564,#11565,#11566,
#11567,#11568,#11569,#11570,#11571,#11572,#11573,#11574,#11575,#11576,#11577,
#11578,#11579,#11580,#11581,#11582,#11583,#11584,#11585,#11586,#11587,#11588,
#11589,#11590,#11591,#11592,#11593,#11594,#11595,#11596,#11597,#11598,#11599,
#11600,#11601,#11602,#11603,#11604,#11605,#11606,#11607,#11608,#11609,#11610,
#11611,#11612,#11613,#11614,#11615,#11616,#11617,#11618,#11619,#11620,#11621,
#11622,#11623,#11624,#11625,#11626,#11627));
#2834=EDGE_LOOP('',(#11628));
#2835=EDGE_LOOP('',(#11629,#11630,#11631,#11632));
#2836=EDGE_LOOP('',(#11633,#11634,#11635,#11636));
#2837=EDGE_LOOP('',(#11637,#11638,#11639,#11640));
#2838=EDGE_LOOP('',(#11641));
#2839=EDGE_LOOP('',(#11642));
#2840=EDGE_LOOP('',(#11643));
#2841=EDGE_LOOP('',(#11644));
#2842=EDGE_LOOP('',(#11645));
#2843=EDGE_LOOP('',(#11646,#11647,#11648,#11649));
#2844=EDGE_LOOP('',(#11650,#11651,#11652,#11653));
#2845=EDGE_LOOP('',(#11654,#11655,#11656,#11657));
#2846=EDGE_LOOP('',(#11658));
#2847=EDGE_LOOP('',(#11659));
#2848=EDGE_LOOP('',(#11660,#11661,#11662,#11663));
#2849=EDGE_LOOP('',(#11664,#11665,#11666,#11667));
#2850=EDGE_LOOP('',(#11668,#11669,#11670,#11671));
#2851=EDGE_LOOP('',(#11672));
#2852=EDGE_LOOP('',(#11673,#11674,#11675,#11676));
#2853=EDGE_LOOP('',(#11677,#11678,#11679,#11680));
#2854=EDGE_LOOP('',(#11681,#11682,#11683,#11684));
#2855=EDGE_LOOP('',(#11685,#11686,#11687,#11688));
#2856=EDGE_LOOP('',(#11689,#11690,#11691,#11692));
#2857=EDGE_LOOP('',(#11693,#11694,#11695,#11696));
#2858=EDGE_LOOP('',(#11697,#11698,#11699,#11700,#11701,#11702));
#2859=EDGE_LOOP('',(#11703,#11704,#11705,#11706,#11707,#11708));
#2860=EDGE_LOOP('',(#11709));
#2861=EDGE_LOOP('',(#11710,#11711,#11712,#11713));
#2862=EDGE_LOOP('',(#11714,#11715,#11716,#11717));
#2863=EDGE_LOOP('',(#11718,#11719,#11720,#11721));
#2864=EDGE_LOOP('',(#11722));
#2865=EDGE_LOOP('',(#11723));
#2866=EDGE_LOOP('',(#11724,#11725,#11726,#11727));
#2867=EDGE_LOOP('',(#11728,#11729,#11730,#11731));
#2868=EDGE_LOOP('',(#11732,#11733,#11734,#11735));
#2869=EDGE_LOOP('',(#11736));
#2870=EDGE_LOOP('',(#11737,#11738,#11739,#11740));
#2871=EDGE_LOOP('',(#11741,#11742,#11743,#11744));
#2872=EDGE_LOOP('',(#11745,#11746,#11747,#11748));
#2873=EDGE_LOOP('',(#11749,#11750,#11751,#11752));
#2874=EDGE_LOOP('',(#11753,#11754,#11755,#11756));
#2875=EDGE_LOOP('',(#11757,#11758,#11759,#11760));
#2876=EDGE_LOOP('',(#11761,#11762,#11763,#11764,#11765,#11766));
#2877=EDGE_LOOP('',(#11767,#11768,#11769,#11770,#11771,#11772));
#2878=EDGE_LOOP('',(#11773,#11774,#11775,#11776));
#2879=EDGE_LOOP('',(#11777,#11778,#11779,#11780));
#2880=EDGE_LOOP('',(#11781));
#2881=EDGE_LOOP('',(#11782));
#2882=EDGE_LOOP('',(#11783));
#2883=EDGE_LOOP('',(#11784));
#2884=LINE('',#17897,#4049);
#2885=LINE('',#17903,#4050);
#2886=LINE('',#17909,#4051);
#2887=LINE('',#17915,#4052);
#2888=LINE('',#17921,#4053);
#2889=LINE('',#17927,#4054);
#2890=LINE('',#17932,#4055);
#2891=LINE('',#17934,#4056);
#2892=LINE('',#17936,#4057);
#2893=LINE('',#17937,#4058);
#2894=LINE('',#17940,#4059);
#2895=LINE('',#17942,#4060);
#2896=LINE('',#17943,#4061);
#2897=LINE('',#17946,#4062);
#2898=LINE('',#17948,#4063);
#2899=LINE('',#17949,#4064);
#2900=LINE('',#17951,#4065);
#2901=LINE('',#17952,#4066);
#2902=LINE('',#17959,#4067);
#2903=LINE('',#17961,#4068);
#2904=LINE('',#17963,#4069);
#2905=LINE('',#17964,#4070);
#2906=LINE('',#17967,#4071);
#2907=LINE('',#17969,#4072);
#2908=LINE('',#17970,#4073);
#2909=LINE('',#17973,#4074);
#2910=LINE('',#17975,#4075);
#2911=LINE('',#17976,#4076);
#2912=LINE('',#17978,#4077);
#2913=LINE('',#17979,#4078);
#2914=LINE('',#17986,#4079);
#2915=LINE('',#17988,#4080);
#2916=LINE('',#17990,#4081);
#2917=LINE('',#17991,#4082);
#2918=LINE('',#17994,#4083);
#2919=LINE('',#17996,#4084);
#2920=LINE('',#17997,#4085);
#2921=LINE('',#18000,#4086);
#2922=LINE('',#18002,#4087);
#2923=LINE('',#18003,#4088);
#2924=LINE('',#18005,#4089);
#2925=LINE('',#18006,#4090);
#2926=LINE('',#18014,#4091);
#2927=LINE('',#18021,#4092);
#2928=LINE('',#18027,#4093);
#2929=LINE('',#18029,#4094);
#2930=LINE('',#18031,#4095);
#2931=LINE('',#18032,#4096);
#2932=LINE('',#18036,#4097);
#2933=LINE('',#18038,#4098);
#2934=LINE('',#18040,#4099);
#2935=LINE('',#18041,#4100);
#2936=LINE('',#18046,#4101);
#2937=LINE('',#18048,#4102);
#2938=LINE('',#18050,#4103);
#2939=LINE('',#18057,#4104);
#2940=LINE('',#18062,#4105);
#2941=LINE('',#18065,#4106);
#2942=LINE('',#18067,#4107);
#2943=LINE('',#18068,#4108);
#2944=LINE('',#18070,#4109);
#2945=LINE('',#18072,#4110);
#2946=LINE('',#18077,#4111);
#2947=LINE('',#18084,#4112);
#2948=LINE('',#18090,#4113);
#2949=LINE('',#18092,#4114);
#2950=LINE('',#18094,#4115);
#2951=LINE('',#18095,#4116);
#2952=LINE('',#18099,#4117);
#2953=LINE('',#18101,#4118);
#2954=LINE('',#18103,#4119);
#2955=LINE('',#18104,#4120);
#2956=LINE('',#18109,#4121);
#2957=LINE('',#18111,#4122);
#2958=LINE('',#18113,#4123);
#2959=LINE('',#18115,#4124);
#2960=LINE('',#18121,#4125);
#2961=LINE('',#18123,#4126);
#2962=LINE('',#18125,#4127);
#2963=LINE('',#18127,#4128);
#2964=LINE('',#18134,#4129);
#2965=LINE('',#18139,#4130);
#2966=LINE('',#18142,#4131);
#2967=LINE('',#18144,#4132);
#2968=LINE('',#18145,#4133);
#2969=LINE('',#18147,#4134);
#2970=LINE('',#18149,#4135);
#2971=LINE('',#18152,#4136);
#2972=LINE('',#18154,#4137);
#2973=LINE('',#18155,#4138);
#2974=LINE('',#18159,#4139);
#2975=LINE('',#18189,#4140);
#2976=LINE('',#18236,#4141);
#2977=LINE('',#18238,#4142);
#2978=LINE('',#18244,#4143);
#2979=LINE('',#18248,#4144);
#2980=LINE('',#18253,#4145);
#2981=LINE('',#18254,#4146);
#2982=LINE('',#18257,#4147);
#2983=LINE('',#18258,#4148);
#2984=LINE('',#18260,#4149);
#2985=LINE('',#18267,#4150);
#2986=LINE('',#18271,#4151);
#2987=LINE('',#18278,#4152);
#2988=LINE('',#18282,#4153);
#2989=LINE('',#18300,#4154);
#2990=LINE('',#18330,#4155);
#2991=LINE('',#18377,#4156);
#2992=LINE('',#18381,#4157);
#2993=LINE('',#18385,#4158);
#2994=LINE('',#18389,#4159);
#2995=LINE('',#18395,#4160);
#2996=LINE('',#18399,#4161);
#2997=LINE('',#18406,#4162);
#2998=LINE('',#18408,#4163);
#2999=LINE('',#18410,#4164);
#3000=LINE('',#18411,#4165);
#3001=LINE('',#18415,#4166);
#3002=LINE('',#18417,#4167);
#3003=LINE('',#18419,#4168);
#3004=LINE('',#18420,#4169);
#3005=LINE('',#18423,#4170);
#3006=LINE('',#18425,#4171);
#3007=LINE('',#18427,#4172);
#3008=LINE('',#18429,#4173);
#3009=LINE('',#18430,#4174);
#3010=LINE('',#18433,#4175);
#3011=LINE('',#18435,#4176);
#3012=LINE('',#18437,#4177);
#3013=LINE('',#18439,#4178);
#3014=LINE('',#18440,#4179);
#3015=LINE('',#18458,#4180);
#3016=LINE('',#18464,#4181);
#3017=LINE('',#18469,#4182);
#3018=LINE('',#18471,#4183);
#3019=LINE('',#18473,#4184);
#3020=LINE('',#18474,#4185);
#3021=LINE('',#18478,#4186);
#3022=LINE('',#18480,#4187);
#3023=LINE('',#18482,#4188);
#3024=LINE('',#18483,#4189);
#3025=LINE('',#18486,#4190);
#3026=LINE('',#18488,#4191);
#3027=LINE('',#18489,#4192);
#3028=LINE('',#18492,#4193);
#3029=LINE('',#18494,#4194);
#3030=LINE('',#18495,#4195);
#3031=LINE('',#18498,#4196);
#3032=LINE('',#18500,#4197);
#3033=LINE('',#18501,#4198);
#3034=LINE('',#18504,#4199);
#3035=LINE('',#18506,#4200);
#3036=LINE('',#18507,#4201);
#3037=LINE('',#18511,#4202);
#3038=LINE('',#18513,#4203);
#3039=LINE('',#18514,#4204);
#3040=LINE('',#18519,#4205);
#3041=LINE('',#18520,#4206);
#3042=LINE('',#18523,#4207);
#3043=LINE('',#18524,#4208);
#3044=LINE('',#18526,#4209);
#3045=LINE('',#18532,#4210);
#3046=LINE('',#18534,#4211);
#3047=LINE('',#18536,#4212);
#3048=LINE('',#18537,#4213);
#3049=LINE('',#18541,#4214);
#3050=LINE('',#18543,#4215);
#3051=LINE('',#18545,#4216);
#3052=LINE('',#18546,#4217);
#3053=LINE('',#18549,#4218);
#3054=LINE('',#18551,#4219);
#3055=LINE('',#18553,#4220);
#3056=LINE('',#18555,#4221);
#3057=LINE('',#18556,#4222);
#3058=LINE('',#18559,#4223);
#3059=LINE('',#18561,#4224);
#3060=LINE('',#18563,#4225);
#3061=LINE('',#18565,#4226);
#3062=LINE('',#18566,#4227);
#3063=LINE('',#18584,#4228);
#3064=LINE('',#18590,#4229);
#3065=LINE('',#18595,#4230);
#3066=LINE('',#18597,#4231);
#3067=LINE('',#18599,#4232);
#3068=LINE('',#18600,#4233);
#3069=LINE('',#18604,#4234);
#3070=LINE('',#18606,#4235);
#3071=LINE('',#18608,#4236);
#3072=LINE('',#18609,#4237);
#3073=LINE('',#18612,#4238);
#3074=LINE('',#18614,#4239);
#3075=LINE('',#18615,#4240);
#3076=LINE('',#18618,#4241);
#3077=LINE('',#18620,#4242);
#3078=LINE('',#18621,#4243);
#3079=LINE('',#18624,#4244);
#3080=LINE('',#18626,#4245);
#3081=LINE('',#18627,#4246);
#3082=LINE('',#18630,#4247);
#3083=LINE('',#18632,#4248);
#3084=LINE('',#18633,#4249);
#3085=LINE('',#18637,#4250);
#3086=LINE('',#18639,#4251);
#3087=LINE('',#18640,#4252);
#3088=LINE('',#18645,#4253);
#3089=LINE('',#18646,#4254);
#3090=LINE('',#18649,#4255);
#3091=LINE('',#18650,#4256);
#3092=LINE('',#18652,#4257);
#3093=LINE('',#18658,#4258);
#3094=LINE('',#18660,#4259);
#3095=LINE('',#18662,#4260);
#3096=LINE('',#18663,#4261);
#3097=LINE('',#18666,#4262);
#3098=LINE('',#18668,#4263);
#3099=LINE('',#18669,#4264);
#3100=LINE('',#18672,#4265);
#3101=LINE('',#18673,#4266);
#3102=LINE('',#18680,#4267);
#3103=LINE('',#18681,#4268);
#3104=LINE('',#18683,#4269);
#3105=LINE('',#18692,#4270);
#3106=LINE('',#18722,#4271);
#3107=LINE('',#18769,#4272);
#3108=LINE('',#18771,#4273);
#3109=LINE('',#18775,#4274);
#3110=LINE('',#18778,#4275);
#3111=LINE('',#18786,#4276);
#3112=LINE('',#18792,#4277);
#3113=LINE('',#18798,#4278);
#3114=LINE('',#18804,#4279);
#3115=LINE('',#18810,#4280);
#3116=LINE('',#18816,#4281);
#3117=LINE('',#18822,#4282);
#3118=LINE('',#18827,#4283);
#3119=LINE('',#18829,#4284);
#3120=LINE('',#18831,#4285);
#3121=LINE('',#18832,#4286);
#3122=LINE('',#18836,#4287);
#3123=LINE('',#18838,#4288);
#3124=LINE('',#18840,#4289);
#3125=LINE('',#18841,#4290);
#3126=LINE('',#18844,#4291);
#3127=LINE('',#18846,#4292);
#3128=LINE('',#18847,#4293);
#3129=LINE('',#18850,#4294);
#3130=LINE('',#18852,#4295);
#3131=LINE('',#18853,#4296);
#3132=LINE('',#18856,#4297);
#3133=LINE('',#18858,#4298);
#3134=LINE('',#18859,#4299);
#3135=LINE('',#18860,#4300);
#3136=LINE('',#18863,#4301);
#3137=LINE('',#18864,#4302);
#3138=LINE('',#18867,#4303);
#3139=LINE('',#18868,#4304);
#3140=LINE('',#18869,#4305);
#3141=LINE('',#18871,#4306);
#3142=LINE('',#18879,#4307);
#3143=LINE('',#18885,#4308);
#3144=LINE('',#18891,#4309);
#3145=LINE('',#18897,#4310);
#3146=LINE('',#18903,#4311);
#3147=LINE('',#18910,#4312);
#3148=LINE('',#18916,#4313);
#3149=LINE('',#18925,#4314);
#3150=LINE('',#18931,#4315);
#3151=LINE('',#18937,#4316);
#3152=LINE('',#18943,#4317);
#3153=LINE('',#18949,#4318);
#3154=LINE('',#18957,#4319);
#3155=LINE('',#18962,#4320);
#3156=LINE('',#18971,#4321);
#3157=LINE('',#18977,#4322);
#3158=LINE('',#18983,#4323);
#3159=LINE('',#18989,#4324);
#3160=LINE('',#18995,#4325);
#3161=LINE('',#19001,#4326);
#3162=LINE('',#19007,#4327);
#3163=LINE('',#19012,#4328);
#3164=LINE('',#19014,#4329);
#3165=LINE('',#19016,#4330);
#3166=LINE('',#19017,#4331);
#3167=LINE('',#19021,#4332);
#3168=LINE('',#19023,#4333);
#3169=LINE('',#19025,#4334);
#3170=LINE('',#19026,#4335);
#3171=LINE('',#19029,#4336);
#3172=LINE('',#19031,#4337);
#3173=LINE('',#19032,#4338);
#3174=LINE('',#19035,#4339);
#3175=LINE('',#19037,#4340);
#3176=LINE('',#19038,#4341);
#3177=LINE('',#19041,#4342);
#3178=LINE('',#19043,#4343);
#3179=LINE('',#19044,#4344);
#3180=LINE('',#19045,#4345);
#3181=LINE('',#19048,#4346);
#3182=LINE('',#19049,#4347);
#3183=LINE('',#19052,#4348);
#3184=LINE('',#19053,#4349);
#3185=LINE('',#19054,#4350);
#3186=LINE('',#19056,#4351);
#3187=LINE('',#19064,#4352);
#3188=LINE('',#19070,#4353);
#3189=LINE('',#19076,#4354);
#3190=LINE('',#19082,#4355);
#3191=LINE('',#19088,#4356);
#3192=LINE('',#19095,#4357);
#3193=LINE('',#19101,#4358);
#3194=LINE('',#19110,#4359);
#3195=LINE('',#19116,#4360);
#3196=LINE('',#19122,#4361);
#3197=LINE('',#19128,#4362);
#3198=LINE('',#19134,#4363);
#3199=LINE('',#19142,#4364);
#3200=LINE('',#19147,#4365);
#3201=LINE('',#19159,#4366);
#3202=LINE('',#19162,#4367);
#3203=LINE('',#19178,#4368);
#3204=LINE('',#19184,#4369);
#3205=LINE('',#19188,#4370);
#3206=LINE('',#19194,#4371);
#3207=LINE('',#19199,#4372);
#3208=LINE('',#19214,#4373);
#3209=LINE('',#19223,#4374);
#3210=LINE('',#19227,#4375);
#3211=LINE('',#19231,#4376);
#3212=LINE('',#19234,#4377);
#3213=LINE('',#19370,#4378);
#3214=LINE('',#19623,#4379);
#3215=LINE('',#19665,#4380);
#3216=LINE('',#19670,#4381);
#3217=LINE('',#19679,#4382);
#3218=LINE('',#19684,#4383);
#3219=LINE('',#19694,#4384);
#3220=LINE('',#19696,#4385);
#3221=LINE('',#19698,#4386);
#3222=LINE('',#19699,#4387);
#3223=LINE('',#19702,#4388);
#3224=LINE('',#19704,#4389);
#3225=LINE('',#19705,#4390);
#3226=LINE('',#19708,#4391);
#3227=LINE('',#19710,#4392);
#3228=LINE('',#19711,#4393);
#3229=LINE('',#19714,#4394);
#3230=LINE('',#19716,#4395);
#3231=LINE('',#19717,#4396);
#3232=LINE('',#19720,#4397);
#3233=LINE('',#19722,#4398);
#3234=LINE('',#19723,#4399);
#3235=LINE('',#19725,#4400);
#3236=LINE('',#19726,#4401);
#3237=LINE('',#19738,#4402);
#3238=LINE('',#19742,#4403);
#3239=LINE('',#19746,#4404);
#3240=LINE('',#19753,#4405);
#3241=LINE('',#19755,#4406);
#3242=LINE('',#19762,#4407);
#3243=LINE('',#19768,#4408);
#3244=LINE('',#19770,#4409);
#3245=LINE('',#19772,#4410);
#3246=LINE('',#19773,#4411);
#3247=LINE('',#19777,#4412);
#3248=LINE('',#19779,#4413);
#3249=LINE('',#19781,#4414);
#3250=LINE('',#19782,#4415);
#3251=LINE('',#19787,#4416);
#3252=LINE('',#19789,#4417);
#3253=LINE('',#19790,#4418);
#3254=LINE('',#19796,#4419);
#3255=LINE('',#19798,#4420);
#3256=LINE('',#19799,#4421);
#3257=LINE('',#19803,#4422);
#3258=LINE('',#19805,#4423);
#3259=LINE('',#19806,#4424);
#3260=LINE('',#19809,#4425);
#3261=LINE('',#19811,#4426);
#3262=LINE('',#19812,#4427);
#3263=LINE('',#19815,#4428);
#3264=LINE('',#19817,#4429);
#3265=LINE('',#19818,#4430);
#3266=LINE('',#19821,#4431);
#3267=LINE('',#19823,#4432);
#3268=LINE('',#19824,#4433);
#3269=LINE('',#19827,#4434);
#3270=LINE('',#19829,#4435);
#3271=LINE('',#19830,#4436);
#3272=LINE('',#19833,#4437);
#3273=LINE('',#19835,#4438);
#3274=LINE('',#19836,#4439);
#3275=LINE('',#19839,#4440);
#3276=LINE('',#19841,#4441);
#3277=LINE('',#19842,#4442);
#3278=LINE('',#19845,#4443);
#3279=LINE('',#19847,#4444);
#3280=LINE('',#19848,#4445);
#3281=LINE('',#19851,#4446);
#3282=LINE('',#19853,#4447);
#3283=LINE('',#19854,#4448);
#3284=LINE('',#19857,#4449);
#3285=LINE('',#19859,#4450);
#3286=LINE('',#19860,#4451);
#3287=LINE('',#19863,#4452);
#3288=LINE('',#19865,#4453);
#3289=LINE('',#19866,#4454);
#3290=LINE('',#19869,#4455);
#3291=LINE('',#19871,#4456);
#3292=LINE('',#19872,#4457);
#3293=LINE('',#19875,#4458);
#3294=LINE('',#19877,#4459);
#3295=LINE('',#19878,#4460);
#3296=LINE('',#19881,#4461);
#3297=LINE('',#19883,#4462);
#3298=LINE('',#19884,#4463);
#3299=LINE('',#19887,#4464);
#3300=LINE('',#19889,#4465);
#3301=LINE('',#19890,#4466);
#3302=LINE('',#19893,#4467);
#3303=LINE('',#19895,#4468);
#3304=LINE('',#19896,#4469);
#3305=LINE('',#19899,#4470);
#3306=LINE('',#19901,#4471);
#3307=LINE('',#19902,#4472);
#3308=LINE('',#19905,#4473);
#3309=LINE('',#19907,#4474);
#3310=LINE('',#19908,#4475);
#3311=LINE('',#19911,#4476);
#3312=LINE('',#19913,#4477);
#3313=LINE('',#19914,#4478);
#3314=LINE('',#19917,#4479);
#3315=LINE('',#19919,#4480);
#3316=LINE('',#19920,#4481);
#3317=LINE('',#19923,#4482);
#3318=LINE('',#19925,#4483);
#3319=LINE('',#19926,#4484);
#3320=LINE('',#19929,#4485);
#3321=LINE('',#19931,#4486);
#3322=LINE('',#19932,#4487);
#3323=LINE('',#19935,#4488);
#3324=LINE('',#19937,#4489);
#3325=LINE('',#19938,#4490);
#3326=LINE('',#19941,#4491);
#3327=LINE('',#19943,#4492);
#3328=LINE('',#19944,#4493);
#3329=LINE('',#19947,#4494);
#3330=LINE('',#19949,#4495);
#3331=LINE('',#19950,#4496);
#3332=LINE('',#19953,#4497);
#3333=LINE('',#19955,#4498);
#3334=LINE('',#19956,#4499);
#3335=LINE('',#19959,#4500);
#3336=LINE('',#19961,#4501);
#3337=LINE('',#19962,#4502);
#3338=LINE('',#19965,#4503);
#3339=LINE('',#19967,#4504);
#3340=LINE('',#19968,#4505);
#3341=LINE('',#19971,#4506);
#3342=LINE('',#19973,#4507);
#3343=LINE('',#19974,#4508);
#3344=LINE('',#19977,#4509);
#3345=LINE('',#19979,#4510);
#3346=LINE('',#19980,#4511);
#3347=LINE('',#19983,#4512);
#3348=LINE('',#19985,#4513);
#3349=LINE('',#19986,#4514);
#3350=LINE('',#19989,#4515);
#3351=LINE('',#19991,#4516);
#3352=LINE('',#19992,#4517);
#3353=LINE('',#19995,#4518);
#3354=LINE('',#19997,#4519);
#3355=LINE('',#19998,#4520);
#3356=LINE('',#20001,#4521);
#3357=LINE('',#20003,#4522);
#3358=LINE('',#20004,#4523);
#3359=LINE('',#20007,#4524);
#3360=LINE('',#20009,#4525);
#3361=LINE('',#20010,#4526);
#3362=LINE('',#20013,#4527);
#3363=LINE('',#20015,#4528);
#3364=LINE('',#20016,#4529);
#3365=LINE('',#20019,#4530);
#3366=LINE('',#20021,#4531);
#3367=LINE('',#20022,#4532);
#3368=LINE('',#20025,#4533);
#3369=LINE('',#20027,#4534);
#3370=LINE('',#20028,#4535);
#3371=LINE('',#20031,#4536);
#3372=LINE('',#20033,#4537);
#3373=LINE('',#20034,#4538);
#3374=LINE('',#20037,#4539);
#3375=LINE('',#20039,#4540);
#3376=LINE('',#20040,#4541);
#3377=LINE('',#20043,#4542);
#3378=LINE('',#20045,#4543);
#3379=LINE('',#20046,#4544);
#3380=LINE('',#20049,#4545);
#3381=LINE('',#20051,#4546);
#3382=LINE('',#20052,#4547);
#3383=LINE('',#20055,#4548);
#3384=LINE('',#20057,#4549);
#3385=LINE('',#20058,#4550);
#3386=LINE('',#20061,#4551);
#3387=LINE('',#20063,#4552);
#3388=LINE('',#20064,#4553);
#3389=LINE('',#20067,#4554);
#3390=LINE('',#20069,#4555);
#3391=LINE('',#20070,#4556);
#3392=LINE('',#20073,#4557);
#3393=LINE('',#20075,#4558);
#3394=LINE('',#20076,#4559);
#3395=LINE('',#20079,#4560);
#3396=LINE('',#20081,#4561);
#3397=LINE('',#20082,#4562);
#3398=LINE('',#20085,#4563);
#3399=LINE('',#20087,#4564);
#3400=LINE('',#20088,#4565);
#3401=LINE('',#20091,#4566);
#3402=LINE('',#20093,#4567);
#3403=LINE('',#20094,#4568);
#3404=LINE('',#20097,#4569);
#3405=LINE('',#20099,#4570);
#3406=LINE('',#20100,#4571);
#3407=LINE('',#20103,#4572);
#3408=LINE('',#20105,#4573);
#3409=LINE('',#20106,#4574);
#3410=LINE('',#20109,#4575);
#3411=LINE('',#20111,#4576);
#3412=LINE('',#20112,#4577);
#3413=LINE('',#20115,#4578);
#3414=LINE('',#20117,#4579);
#3415=LINE('',#20118,#4580);
#3416=LINE('',#20121,#4581);
#3417=LINE('',#20123,#4582);
#3418=LINE('',#20124,#4583);
#3419=LINE('',#20127,#4584);
#3420=LINE('',#20129,#4585);
#3421=LINE('',#20130,#4586);
#3422=LINE('',#20133,#4587);
#3423=LINE('',#20135,#4588);
#3424=LINE('',#20136,#4589);
#3425=LINE('',#20139,#4590);
#3426=LINE('',#20141,#4591);
#3427=LINE('',#20142,#4592);
#3428=LINE('',#20145,#4593);
#3429=LINE('',#20147,#4594);
#3430=LINE('',#20148,#4595);
#3431=LINE('',#20151,#4596);
#3432=LINE('',#20153,#4597);
#3433=LINE('',#20154,#4598);
#3434=LINE('',#20157,#4599);
#3435=LINE('',#20159,#4600);
#3436=LINE('',#20160,#4601);
#3437=LINE('',#20163,#4602);
#3438=LINE('',#20165,#4603);
#3439=LINE('',#20166,#4604);
#3440=LINE('',#20169,#4605);
#3441=LINE('',#20171,#4606);
#3442=LINE('',#20172,#4607);
#3443=LINE('',#20175,#4608);
#3444=LINE('',#20177,#4609);
#3445=LINE('',#20178,#4610);
#3446=LINE('',#20181,#4611);
#3447=LINE('',#20183,#4612);
#3448=LINE('',#20184,#4613);
#3449=LINE('',#20187,#4614);
#3450=LINE('',#20189,#4615);
#3451=LINE('',#20190,#4616);
#3452=LINE('',#20193,#4617);
#3453=LINE('',#20195,#4618);
#3454=LINE('',#20196,#4619);
#3455=LINE('',#20199,#4620);
#3456=LINE('',#20201,#4621);
#3457=LINE('',#20202,#4622);
#3458=LINE('',#20205,#4623);
#3459=LINE('',#20207,#4624);
#3460=LINE('',#20208,#4625);
#3461=LINE('',#20211,#4626);
#3462=LINE('',#20213,#4627);
#3463=LINE('',#20214,#4628);
#3464=LINE('',#20217,#4629);
#3465=LINE('',#20219,#4630);
#3466=LINE('',#20220,#4631);
#3467=LINE('',#20223,#4632);
#3468=LINE('',#20225,#4633);
#3469=LINE('',#20226,#4634);
#3470=LINE('',#20229,#4635);
#3471=LINE('',#20231,#4636);
#3472=LINE('',#20232,#4637);
#3473=LINE('',#20235,#4638);
#3474=LINE('',#20237,#4639);
#3475=LINE('',#20238,#4640);
#3476=LINE('',#20241,#4641);
#3477=LINE('',#20243,#4642);
#3478=LINE('',#20244,#4643);
#3479=LINE('',#20247,#4644);
#3480=LINE('',#20249,#4645);
#3481=LINE('',#20250,#4646);
#3482=LINE('',#20253,#4647);
#3483=LINE('',#20255,#4648);
#3484=LINE('',#20256,#4649);
#3485=LINE('',#20259,#4650);
#3486=LINE('',#20261,#4651);
#3487=LINE('',#20262,#4652);
#3488=LINE('',#20265,#4653);
#3489=LINE('',#20267,#4654);
#3490=LINE('',#20268,#4655);
#3491=LINE('',#20271,#4656);
#3492=LINE('',#20273,#4657);
#3493=LINE('',#20274,#4658);
#3494=LINE('',#20277,#4659);
#3495=LINE('',#20279,#4660);
#3496=LINE('',#20280,#4661);
#3497=LINE('',#20283,#4662);
#3498=LINE('',#20285,#4663);
#3499=LINE('',#20286,#4664);
#3500=LINE('',#20289,#4665);
#3501=LINE('',#20291,#4666);
#3502=LINE('',#20292,#4667);
#3503=LINE('',#20295,#4668);
#3504=LINE('',#20297,#4669);
#3505=LINE('',#20298,#4670);
#3506=LINE('',#20301,#4671);
#3507=LINE('',#20303,#4672);
#3508=LINE('',#20304,#4673);
#3509=LINE('',#20307,#4674);
#3510=LINE('',#20309,#4675);
#3511=LINE('',#20310,#4676);
#3512=LINE('',#20313,#4677);
#3513=LINE('',#20315,#4678);
#3514=LINE('',#20316,#4679);
#3515=LINE('',#20319,#4680);
#3516=LINE('',#20321,#4681);
#3517=LINE('',#20322,#4682);
#3518=LINE('',#20325,#4683);
#3519=LINE('',#20327,#4684);
#3520=LINE('',#20328,#4685);
#3521=LINE('',#20331,#4686);
#3522=LINE('',#20333,#4687);
#3523=LINE('',#20334,#4688);
#3524=LINE('',#20337,#4689);
#3525=LINE('',#20339,#4690);
#3526=LINE('',#20340,#4691);
#3527=LINE('',#20343,#4692);
#3528=LINE('',#20345,#4693);
#3529=LINE('',#20346,#4694);
#3530=LINE('',#20349,#4695);
#3531=LINE('',#20351,#4696);
#3532=LINE('',#20352,#4697);
#3533=LINE('',#20355,#4698);
#3534=LINE('',#20357,#4699);
#3535=LINE('',#20358,#4700);
#3536=LINE('',#20361,#4701);
#3537=LINE('',#20363,#4702);
#3538=LINE('',#20364,#4703);
#3539=LINE('',#20367,#4704);
#3540=LINE('',#20369,#4705);
#3541=LINE('',#20370,#4706);
#3542=LINE('',#20373,#4707);
#3543=LINE('',#20375,#4708);
#3544=LINE('',#20376,#4709);
#3545=LINE('',#20379,#4710);
#3546=LINE('',#20381,#4711);
#3547=LINE('',#20382,#4712);
#3548=LINE('',#20385,#4713);
#3549=LINE('',#20387,#4714);
#3550=LINE('',#20388,#4715);
#3551=LINE('',#20391,#4716);
#3552=LINE('',#20393,#4717);
#3553=LINE('',#20394,#4718);
#3554=LINE('',#20397,#4719);
#3555=LINE('',#20399,#4720);
#3556=LINE('',#20400,#4721);
#3557=LINE('',#20403,#4722);
#3558=LINE('',#20405,#4723);
#3559=LINE('',#20406,#4724);
#3560=LINE('',#20409,#4725);
#3561=LINE('',#20411,#4726);
#3562=LINE('',#20412,#4727);
#3563=LINE('',#20415,#4728);
#3564=LINE('',#20417,#4729);
#3565=LINE('',#20418,#4730);
#3566=LINE('',#20421,#4731);
#3567=LINE('',#20423,#4732);
#3568=LINE('',#20424,#4733);
#3569=LINE('',#20427,#4734);
#3570=LINE('',#20429,#4735);
#3571=LINE('',#20430,#4736);
#3572=LINE('',#20433,#4737);
#3573=LINE('',#20435,#4738);
#3574=LINE('',#20436,#4739);
#3575=LINE('',#20439,#4740);
#3576=LINE('',#20441,#4741);
#3577=LINE('',#20442,#4742);
#3578=LINE('',#20445,#4743);
#3579=LINE('',#20447,#4744);
#3580=LINE('',#20448,#4745);
#3581=LINE('',#20451,#4746);
#3582=LINE('',#20453,#4747);
#3583=LINE('',#20454,#4748);
#3584=LINE('',#20457,#4749);
#3585=LINE('',#20459,#4750);
#3586=LINE('',#20460,#4751);
#3587=LINE('',#20463,#4752);
#3588=LINE('',#20465,#4753);
#3589=LINE('',#20466,#4754);
#3590=LINE('',#20469,#4755);
#3591=LINE('',#20471,#4756);
#3592=LINE('',#20472,#4757);
#3593=LINE('',#20475,#4758);
#3594=LINE('',#20477,#4759);
#3595=LINE('',#20478,#4760);
#3596=LINE('',#20481,#4761);
#3597=LINE('',#20483,#4762);
#3598=LINE('',#20484,#4763);
#3599=LINE('',#20487,#4764);
#3600=LINE('',#20489,#4765);
#3601=LINE('',#20490,#4766);
#3602=LINE('',#20493,#4767);
#3603=LINE('',#20495,#4768);
#3604=LINE('',#20496,#4769);
#3605=LINE('',#20499,#4770);
#3606=LINE('',#20501,#4771);
#3607=LINE('',#20502,#4772);
#3608=LINE('',#20505,#4773);
#3609=LINE('',#20507,#4774);
#3610=LINE('',#20508,#4775);
#3611=LINE('',#20511,#4776);
#3612=LINE('',#20513,#4777);
#3613=LINE('',#20514,#4778);
#3614=LINE('',#20517,#4779);
#3615=LINE('',#20519,#4780);
#3616=LINE('',#20520,#4781);
#3617=LINE('',#20523,#4782);
#3618=LINE('',#20525,#4783);
#3619=LINE('',#20526,#4784);
#3620=LINE('',#20529,#4785);
#3621=LINE('',#20531,#4786);
#3622=LINE('',#20532,#4787);
#3623=LINE('',#20535,#4788);
#3624=LINE('',#20537,#4789);
#3625=LINE('',#20538,#4790);
#3626=LINE('',#20541,#4791);
#3627=LINE('',#20543,#4792);
#3628=LINE('',#20544,#4793);
#3629=LINE('',#20547,#4794);
#3630=LINE('',#20549,#4795);
#3631=LINE('',#20550,#4796);
#3632=LINE('',#20553,#4797);
#3633=LINE('',#20555,#4798);
#3634=LINE('',#20556,#4799);
#3635=LINE('',#20559,#4800);
#3636=LINE('',#20561,#4801);
#3637=LINE('',#20562,#4802);
#3638=LINE('',#20565,#4803);
#3639=LINE('',#20567,#4804);
#3640=LINE('',#20568,#4805);
#3641=LINE('',#20571,#4806);
#3642=LINE('',#20573,#4807);
#3643=LINE('',#20574,#4808);
#3644=LINE('',#20577,#4809);
#3645=LINE('',#20579,#4810);
#3646=LINE('',#20580,#4811);
#3647=LINE('',#20583,#4812);
#3648=LINE('',#20585,#4813);
#3649=LINE('',#20586,#4814);
#3650=LINE('',#20589,#4815);
#3651=LINE('',#20591,#4816);
#3652=LINE('',#20592,#4817);
#3653=LINE('',#20595,#4818);
#3654=LINE('',#20597,#4819);
#3655=LINE('',#20598,#4820);
#3656=LINE('',#20601,#4821);
#3657=LINE('',#20603,#4822);
#3658=LINE('',#20604,#4823);
#3659=LINE('',#20607,#4824);
#3660=LINE('',#20609,#4825);
#3661=LINE('',#20610,#4826);
#3662=LINE('',#20613,#4827);
#3663=LINE('',#20615,#4828);
#3664=LINE('',#20616,#4829);
#3665=LINE('',#20619,#4830);
#3666=LINE('',#20621,#4831);
#3667=LINE('',#20622,#4832);
#3668=LINE('',#20625,#4833);
#3669=LINE('',#20627,#4834);
#3670=LINE('',#20628,#4835);
#3671=LINE('',#20631,#4836);
#3672=LINE('',#20633,#4837);
#3673=LINE('',#20634,#4838);
#3674=LINE('',#20637,#4839);
#3675=LINE('',#20639,#4840);
#3676=LINE('',#20640,#4841);
#3677=LINE('',#20643,#4842);
#3678=LINE('',#20645,#4843);
#3679=LINE('',#20646,#4844);
#3680=LINE('',#20649,#4845);
#3681=LINE('',#20651,#4846);
#3682=LINE('',#20652,#4847);
#3683=LINE('',#20655,#4848);
#3684=LINE('',#20657,#4849);
#3685=LINE('',#20658,#4850);
#3686=LINE('',#20661,#4851);
#3687=LINE('',#20663,#4852);
#3688=LINE('',#20664,#4853);
#3689=LINE('',#20667,#4854);
#3690=LINE('',#20669,#4855);
#3691=LINE('',#20670,#4856);
#3692=LINE('',#20673,#4857);
#3693=LINE('',#20675,#4858);
#3694=LINE('',#20676,#4859);
#3695=LINE('',#20679,#4860);
#3696=LINE('',#20681,#4861);
#3697=LINE('',#20682,#4862);
#3698=LINE('',#20685,#4863);
#3699=LINE('',#20687,#4864);
#3700=LINE('',#20688,#4865);
#3701=LINE('',#20691,#4866);
#3702=LINE('',#20693,#4867);
#3703=LINE('',#20694,#4868);
#3704=LINE('',#20697,#4869);
#3705=LINE('',#20699,#4870);
#3706=LINE('',#20700,#4871);
#3707=LINE('',#20703,#4872);
#3708=LINE('',#20705,#4873);
#3709=LINE('',#20706,#4874);
#3710=LINE('',#20709,#4875);
#3711=LINE('',#20711,#4876);
#3712=LINE('',#20712,#4877);
#3713=LINE('',#20715,#4878);
#3714=LINE('',#20717,#4879);
#3715=LINE('',#20718,#4880);
#3716=LINE('',#20721,#4881);
#3717=LINE('',#20723,#4882);
#3718=LINE('',#20724,#4883);
#3719=LINE('',#20727,#4884);
#3720=LINE('',#20729,#4885);
#3721=LINE('',#20730,#4886);
#3722=LINE('',#20733,#4887);
#3723=LINE('',#20735,#4888);
#3724=LINE('',#20736,#4889);
#3725=LINE('',#20739,#4890);
#3726=LINE('',#20741,#4891);
#3727=LINE('',#20742,#4892);
#3728=LINE('',#20745,#4893);
#3729=LINE('',#20747,#4894);
#3730=LINE('',#20748,#4895);
#3731=LINE('',#20751,#4896);
#3732=LINE('',#20753,#4897);
#3733=LINE('',#20754,#4898);
#3734=LINE('',#20757,#4899);
#3735=LINE('',#20759,#4900);
#3736=LINE('',#20760,#4901);
#3737=LINE('',#20762,#4902);
#3738=LINE('',#20763,#4903);
#3739=LINE('',#20769,#4904);
#3740=LINE('',#20771,#4905);
#3741=LINE('',#20779,#4906);
#3742=LINE('',#20803,#4907);
#3743=LINE('',#20848,#4908);
#3744=LINE('',#20853,#4909);
#3745=LINE('',#20859,#4910);
#3746=LINE('',#20866,#4911);
#3747=LINE('',#20875,#4912);
#3748=LINE('',#20884,#4913);
#3749=LINE('',#20929,#4914);
#3750=LINE('',#20970,#4915);
#3751=LINE('',#20972,#4916);
#3752=LINE('',#20974,#4917);
#3753=LINE('',#20975,#4918);
#3754=LINE('',#20979,#4919);
#3755=LINE('',#20981,#4920);
#3756=LINE('',#20983,#4921);
#3757=LINE('',#20984,#4922);
#3758=LINE('',#20987,#4923);
#3759=LINE('',#20989,#4924);
#3760=LINE('',#20990,#4925);
#3761=LINE('',#20993,#4926);
#3762=LINE('',#20995,#4927);
#3763=LINE('',#20996,#4928);
#3764=LINE('',#21009,#4929);
#3765=LINE('',#21011,#4930);
#3766=LINE('',#21013,#4931);
#3767=LINE('',#21014,#4932);
#3768=LINE('',#21017,#4933);
#3769=LINE('',#21019,#4934);
#3770=LINE('',#21020,#4935);
#3771=LINE('',#21023,#4936);
#3772=LINE('',#21025,#4937);
#3773=LINE('',#21026,#4938);
#3774=LINE('',#21029,#4939);
#3775=LINE('',#21031,#4940);
#3776=LINE('',#21032,#4941);
#3777=LINE('',#21035,#4942);
#3778=LINE('',#21037,#4943);
#3779=LINE('',#21038,#4944);
#3780=LINE('',#21040,#4945);
#3781=LINE('',#21041,#4946);
#3782=LINE('',#21049,#4947);
#3783=LINE('',#21053,#4948);
#3784=LINE('',#21057,#4949);
#3785=LINE('',#21071,#4950);
#3786=LINE('',#21078,#4951);
#3787=LINE('',#21084,#4952);
#3788=LINE('',#21086,#4953);
#3789=LINE('',#21088,#4954);
#3790=LINE('',#21089,#4955);
#3791=LINE('',#21094,#4956);
#3792=LINE('',#21095,#4957);
#3793=LINE('',#21098,#4958);
#3794=LINE('',#21099,#4959);
#3795=LINE('',#21102,#4960);
#3796=LINE('',#21103,#4961);
#3797=LINE('',#21109,#4962);
#3798=LINE('',#21111,#4963);
#3799=LINE('',#21113,#4964);
#3800=LINE('',#21114,#4965);
#3801=LINE('',#21119,#4966);
#3802=LINE('',#21120,#4967);
#3803=LINE('',#21123,#4968);
#3804=LINE('',#21124,#4969);
#3805=LINE('',#21127,#4970);
#3806=LINE('',#21128,#4971);
#3807=LINE('',#21135,#4972);
#3808=LINE('',#21144,#4973);
#3809=LINE('',#21150,#4974);
#3810=LINE('',#21159,#4975);
#3811=LINE('',#21165,#4976);
#3812=LINE('',#21174,#4977);
#3813=LINE('',#21180,#4978);
#3814=LINE('',#21189,#4979);
#3815=LINE('',#21195,#4980);
#3816=LINE('',#21203,#4981);
#3817=LINE('',#21205,#4982);
#3818=LINE('',#21207,#4983);
#3819=LINE('',#21208,#4984);
#3820=LINE('',#21211,#4985);
#3821=LINE('',#21213,#4986);
#3822=LINE('',#21214,#4987);
#3823=LINE('',#21217,#4988);
#3824=LINE('',#21219,#4989);
#3825=LINE('',#21220,#4990);
#3826=LINE('',#21222,#4991);
#3827=LINE('',#21223,#4992);
#3828=LINE('',#21230,#4993);
#3829=LINE('',#21232,#4994);
#3830=LINE('',#21234,#4995);
#3831=LINE('',#21235,#4996);
#3832=LINE('',#21238,#4997);
#3833=LINE('',#21240,#4998);
#3834=LINE('',#21241,#4999);
#3835=LINE('',#21244,#5000);
#3836=LINE('',#21246,#5001);
#3837=LINE('',#21247,#5002);
#3838=LINE('',#21249,#5003);
#3839=LINE('',#21250,#5004);
#3840=LINE('',#21258,#5005);
#3841=LINE('',#21263,#5006);
#3842=LINE('',#21265,#5007);
#3843=LINE('',#21267,#5008);
#3844=LINE('',#21268,#5009);
#3845=LINE('',#21271,#5010);
#3846=LINE('',#21273,#5011);
#3847=LINE('',#21274,#5012);
#3848=LINE('',#21277,#5013);
#3849=LINE('',#21279,#5014);
#3850=LINE('',#21280,#5015);
#3851=LINE('',#21290,#5016);
#3852=LINE('',#21294,#5017);
#3853=LINE('',#21298,#5018);
#3854=LINE('',#21300,#5019);
#3855=LINE('',#21301,#5020);
#3856=LINE('',#21304,#5021);
#3857=LINE('',#21308,#5022);
#3858=LINE('',#21309,#5023);
#3859=LINE('',#21314,#5024);
#3860=LINE('',#21322,#5025);
#3861=LINE('',#21328,#5026);
#3862=LINE('',#21337,#5027);
#3863=LINE('',#21343,#5028);
#3864=LINE('',#21352,#5029);
#3865=LINE('',#21358,#5030);
#3866=LINE('',#21366,#5031);
#3867=LINE('',#21368,#5032);
#3868=LINE('',#21370,#5033);
#3869=LINE('',#21371,#5034);
#3870=LINE('',#21374,#5035);
#3871=LINE('',#21376,#5036);
#3872=LINE('',#21377,#5037);
#3873=LINE('',#21380,#5038);
#3874=LINE('',#21382,#5039);
#3875=LINE('',#21383,#5040);
#3876=LINE('',#21460,#5041);
#3877=LINE('',#21606,#5042);
#3878=LINE('',#21752,#5043);
#3879=LINE('',#21898,#5044);
#3880=LINE('',#22044,#5045);
#3881=LINE('',#22190,#5046);
#3882=LINE('',#22336,#5047);
#3883=LINE('',#22482,#5048);
#3884=LINE('',#22628,#5049);
#3885=LINE('',#22774,#5050);
#3886=LINE('',#22920,#5051);
#3887=LINE('',#23066,#5052);
#3888=LINE('',#23212,#5053);
#3889=LINE('',#23358,#5054);
#3890=LINE('',#23504,#5055);
#3891=LINE('',#23650,#5056);
#3892=LINE('',#23796,#5057);
#3893=LINE('',#23942,#5058);
#3894=LINE('',#24088,#5059);
#3895=LINE('',#24234,#5060);
#3896=LINE('',#24312,#5061);
#3897=LINE('',#24456,#5062);
#3898=LINE('',#24528,#5063);
#3899=LINE('',#24531,#5064);
#3900=LINE('',#24532,#5065);
#3901=LINE('',#24744,#5066);
#3902=LINE('',#24748,#5067);
#3903=LINE('',#24960,#5068);
#3904=LINE('',#24963,#5069);
#3905=LINE('',#24964,#5070);
#3906=LINE('',#25176,#5071);
#3907=LINE('',#25180,#5072);
#3908=LINE('',#25392,#5073);
#3909=LINE('',#25395,#5074);
#3910=LINE('',#25396,#5075);
#3911=LINE('',#25608,#5076);
#3912=LINE('',#25612,#5077);
#3913=LINE('',#25824,#5078);
#3914=LINE('',#25827,#5079);
#3915=LINE('',#25828,#5080);
#3916=LINE('',#26040,#5081);
#3917=LINE('',#26044,#5082);
#3918=LINE('',#26256,#5083);
#3919=LINE('',#26259,#5084);
#3920=LINE('',#26260,#5085);
#3921=LINE('',#26472,#5086);
#3922=LINE('',#26476,#5087);
#3923=LINE('',#26688,#5088);
#3924=LINE('',#26691,#5089);
#3925=LINE('',#26692,#5090);
#3926=LINE('',#26904,#5091);
#3927=LINE('',#26908,#5092);
#3928=LINE('',#27120,#5093);
#3929=LINE('',#27123,#5094);
#3930=LINE('',#27124,#5095);
#3931=LINE('',#27336,#5096);
#3932=LINE('',#27340,#5097);
#3933=LINE('',#27552,#5098);
#3934=LINE('',#27555,#5099);
#3935=LINE('',#27556,#5100);
#3936=LINE('',#27768,#5101);
#3937=LINE('',#27772,#5102);
#3938=LINE('',#27984,#5103);
#3939=LINE('',#27987,#5104);
#3940=LINE('',#27988,#5105);
#3941=LINE('',#28200,#5106);
#3942=LINE('',#28204,#5107);
#3943=LINE('',#28416,#5108);
#3944=LINE('',#28419,#5109);
#3945=LINE('',#28420,#5110);
#3946=LINE('',#28632,#5111);
#3947=LINE('',#28636,#5112);
#3948=LINE('',#28848,#5113);
#3949=LINE('',#28851,#5114);
#3950=LINE('',#28852,#5115);
#3951=LINE('',#29064,#5116);
#3952=LINE('',#29068,#5117);
#3953=LINE('',#29280,#5118);
#3954=LINE('',#29283,#5119);
#3955=LINE('',#29284,#5120);
#3956=LINE('',#29496,#5121);
#3957=LINE('',#29500,#5122);
#3958=LINE('',#29712,#5123);
#3959=LINE('',#29715,#5124);
#3960=LINE('',#29716,#5125);
#3961=LINE('',#29928,#5126);
#3962=LINE('',#29932,#5127);
#3963=LINE('',#30144,#5128);
#3964=LINE('',#30147,#5129);
#3965=LINE('',#30148,#5130);
#3966=LINE('',#30360,#5131);
#3967=LINE('',#30364,#5132);
#3968=LINE('',#30576,#5133);
#3969=LINE('',#30579,#5134);
#3970=LINE('',#30580,#5135);
#3971=LINE('',#30792,#5136);
#3972=LINE('',#30796,#5137);
#3973=LINE('',#31008,#5138);
#3974=LINE('',#31011,#5139);
#3975=LINE('',#31012,#5140);
#3976=LINE('',#31224,#5141);
#3977=LINE('',#31228,#5142);
#3978=LINE('',#31440,#5143);
#3979=LINE('',#31443,#5144);
#3980=LINE('',#31444,#5145);
#3981=LINE('',#31656,#5146);
#3982=LINE('',#31660,#5147);
#3983=LINE('',#31872,#5148);
#3984=LINE('',#31875,#5149);
#3985=LINE('',#31876,#5150);
#3986=LINE('',#32088,#5151);
#3987=LINE('',#32092,#5152);
#3988=LINE('',#32304,#5153);
#3989=LINE('',#32307,#5154);
#3990=LINE('',#32308,#5155);
#3991=LINE('',#32520,#5156);
#3992=LINE('',#32524,#5157);
#3993=LINE('',#32736,#5158);
#3994=LINE('',#32739,#5159);
#3995=LINE('',#32740,#5160);
#3996=LINE('',#32952,#5161);
#3997=LINE('',#32961,#5162);
#3998=LINE('',#32967,#5163);
#3999=LINE('',#32978,#5164);
#4000=LINE('',#32982,#5165);
#4001=LINE('',#32986,#5166);
#4002=LINE('',#32993,#5167);
#4003=LINE('',#32997,#5168);
#4004=LINE('',#33001,#5169);
#4005=LINE('',#33006,#5170);
#4006=LINE('',#33008,#5171);
#4007=LINE('',#33010,#5172);
#4008=LINE('',#33011,#5173);
#4009=LINE('',#33014,#5174);
#4010=LINE('',#33016,#5175);
#4011=LINE('',#33017,#5176);
#4012=LINE('',#33020,#5177);
#4013=LINE('',#33022,#5178);
#4014=LINE('',#33023,#5179);
#4015=LINE('',#33026,#5180);
#4016=LINE('',#33028,#5181);
#4017=LINE('',#33029,#5182);
#4018=LINE('',#33032,#5183);
#4019=LINE('',#33034,#5184);
#4020=LINE('',#33035,#5185);
#4021=LINE('',#33037,#5186);
#4022=LINE('',#33038,#5187);
#4023=LINE('',#33048,#5188);
#4024=LINE('',#33052,#5189);
#4025=LINE('',#33056,#5190);
#4026=LINE('',#33063,#5191);
#4027=LINE('',#33067,#5192);
#4028=LINE('',#33071,#5193);
#4029=LINE('',#33076,#5194);
#4030=LINE('',#33078,#5195);
#4031=LINE('',#33080,#5196);
#4032=LINE('',#33081,#5197);
#4033=LINE('',#33084,#5198);
#4034=LINE('',#33086,#5199);
#4035=LINE('',#33087,#5200);
#4036=LINE('',#33090,#5201);
#4037=LINE('',#33092,#5202);
#4038=LINE('',#33093,#5203);
#4039=LINE('',#33096,#5204);
#4040=LINE('',#33098,#5205);
#4041=LINE('',#33099,#5206);
#4042=LINE('',#33102,#5207);
#4043=LINE('',#33104,#5208);
#4044=LINE('',#33105,#5209);
#4045=LINE('',#33107,#5210);
#4046=LINE('',#33108,#5211);
#4047=LINE('',#33181,#5212);
#4048=LINE('',#33187,#5213);
#4049=VECTOR('',#14377,0.165);
#4050=VECTOR('',#14384,0.165);
#4051=VECTOR('',#14391,0.165);
#4052=VECTOR('',#14398,0.165);
#4053=VECTOR('',#14405,0.165);
#4054=VECTOR('',#14412,0.165);
#4055=VECTOR('',#14417,1.);
#4056=VECTOR('',#14418,1.);
#4057=VECTOR('',#14419,1.);
#4058=VECTOR('',#14420,1.);
#4059=VECTOR('',#14423,1.);
#4060=VECTOR('',#14424,1.);
#4061=VECTOR('',#14425,1.);
#4062=VECTOR('',#14428,1.);
#4063=VECTOR('',#14429,1.);
#4064=VECTOR('',#14430,1.);
#4065=VECTOR('',#14433,1.);
#4066=VECTOR('',#14434,1.);
#4067=VECTOR('',#14443,1.);
#4068=VECTOR('',#14444,1.);
#4069=VECTOR('',#14445,1.);
#4070=VECTOR('',#14446,1.);
#4071=VECTOR('',#14449,1.);
#4072=VECTOR('',#14450,1.);
#4073=VECTOR('',#14451,1.);
#4074=VECTOR('',#14454,1.);
#4075=VECTOR('',#14455,1.);
#4076=VECTOR('',#14456,1.);
#4077=VECTOR('',#14459,1.);
#4078=VECTOR('',#14460,1.);
#4079=VECTOR('',#14469,1.);
#4080=VECTOR('',#14470,1.);
#4081=VECTOR('',#14471,1.);
#4082=VECTOR('',#14472,1.);
#4083=VECTOR('',#14475,1.);
#4084=VECTOR('',#14476,1.);
#4085=VECTOR('',#14477,1.);
#4086=VECTOR('',#14480,1.);
#4087=VECTOR('',#14481,1.);
#4088=VECTOR('',#14482,1.);
#4089=VECTOR('',#14485,1.);
#4090=VECTOR('',#14486,1.);
#4091=VECTOR('',#14497,0.165);
#4092=VECTOR('',#14506,0.165);
#4093=VECTOR('',#14513,1.);
#4094=VECTOR('',#14514,1.);
#4095=VECTOR('',#14515,1.);
#4096=VECTOR('',#14516,1.);
#4097=VECTOR('',#14519,1.);
#4098=VECTOR('',#14520,1.);
#4099=VECTOR('',#14521,1.);
#4100=VECTOR('',#14522,1.);
#4101=VECTOR('',#14527,1.);
#4102=VECTOR('',#14528,1.);
#4103=VECTOR('',#14529,1.);
#4104=VECTOR('',#14540,1.);
#4105=VECTOR('',#14547,1.);
#4106=VECTOR('',#14550,1.);
#4107=VECTOR('',#14551,1.);
#4108=VECTOR('',#14552,1.);
#4109=VECTOR('',#14555,1.);
#4110=VECTOR('',#14558,1.);
#4111=VECTOR('',#14563,0.165);
#4112=VECTOR('',#14572,0.165);
#4113=VECTOR('',#14579,1.);
#4114=VECTOR('',#14580,1.);
#4115=VECTOR('',#14581,1.);
#4116=VECTOR('',#14582,1.);
#4117=VECTOR('',#14585,1.);
#4118=VECTOR('',#14586,1.);
#4119=VECTOR('',#14587,1.);
#4120=VECTOR('',#14588,1.);
#4121=VECTOR('',#14593,1.);
#4122=VECTOR('',#14594,1.);
#4123=VECTOR('',#14595,1.);
#4124=VECTOR('',#14596,1.);
#4125=VECTOR('',#14601,1.);
#4126=VECTOR('',#14602,1.);
#4127=VECTOR('',#14603,1.);
#4128=VECTOR('',#14604,1.);
#4129=VECTOR('',#14615,1.);
#4130=VECTOR('',#14622,1.);
#4131=VECTOR('',#14625,1.);
#4132=VECTOR('',#14626,1.);
#4133=VECTOR('',#14627,1.);
#4134=VECTOR('',#14630,1.);
#4135=VECTOR('',#14633,1.);
#4136=VECTOR('',#14636,1.);
#4137=VECTOR('',#14637,1.);
#4138=VECTOR('',#14638,1.);
#4139=VECTOR('',#14641,1.);
#4140=VECTOR('',#14648,0.164999999999999);
#4141=VECTOR('',#14651,1.);
#4142=VECTOR('',#14654,1.);
#4143=VECTOR('',#14661,0.605);
#4144=VECTOR('',#14666,1.4);
#4145=VECTOR('',#14673,1.);
#4146=VECTOR('',#14674,1.);
#4147=VECTOR('',#14677,1.);
#4148=VECTOR('',#14678,1.);
#4149=VECTOR('',#14681,1.);
#4150=VECTOR('',#14690,1.);
#4151=VECTOR('',#14693,1.);
#4152=VECTOR('',#14702,1.);
#4153=VECTOR('',#14705,1.);
#4154=VECTOR('',#14728,1.);
#4155=VECTOR('',#14735,0.165);
#4156=VECTOR('',#14738,1.);
#4157=VECTOR('',#14743,0.225);
#4158=VECTOR('',#14748,0.225);
#4159=VECTOR('',#14753,1.4);
#4160=VECTOR('',#14760,0.605);
#4161=VECTOR('',#14765,2.);
#4162=VECTOR('',#14774,1.);
#4163=VECTOR('',#14775,1.);
#4164=VECTOR('',#14776,1.);
#4165=VECTOR('',#14777,1.);
#4166=VECTOR('',#14780,1.);
#4167=VECTOR('',#14781,1.);
#4168=VECTOR('',#14782,1.);
#4169=VECTOR('',#14783,1.);
#4170=VECTOR('',#14786,1.);
#4171=VECTOR('',#14787,1.);
#4172=VECTOR('',#14788,1.);
#4173=VECTOR('',#14789,1.);
#4174=VECTOR('',#14790,1.);
#4175=VECTOR('',#14793,1.);
#4176=VECTOR('',#14794,1.);
#4177=VECTOR('',#14795,1.);
#4178=VECTOR('',#14796,1.);
#4179=VECTOR('',#14797,1.);
#4180=VECTOR('',#14828,0.225);
#4181=VECTOR('',#14835,0.225);
#4182=VECTOR('',#14840,1.);
#4183=VECTOR('',#14841,1.);
#4184=VECTOR('',#14842,1.);
#4185=VECTOR('',#14843,1.);
#4186=VECTOR('',#14846,1.);
#4187=VECTOR('',#14847,1.);
#4188=VECTOR('',#14848,1.);
#4189=VECTOR('',#14849,1.);
#4190=VECTOR('',#14852,1.);
#4191=VECTOR('',#14853,1.);
#4192=VECTOR('',#14854,1.);
#4193=VECTOR('',#14857,1.);
#4194=VECTOR('',#14858,1.);
#4195=VECTOR('',#14859,1.);
#4196=VECTOR('',#14862,1.);
#4197=VECTOR('',#14863,1.);
#4198=VECTOR('',#14864,1.);
#4199=VECTOR('',#14867,1.);
#4200=VECTOR('',#14868,1.);
#4201=VECTOR('',#14869,1.);
#4202=VECTOR('',#14874,1.);
#4203=VECTOR('',#14875,1.);
#4204=VECTOR('',#14876,1.);
#4205=VECTOR('',#14883,1.);
#4206=VECTOR('',#14884,1.);
#4207=VECTOR('',#14887,1.);
#4208=VECTOR('',#14888,1.);
#4209=VECTOR('',#14891,1.);
#4210=VECTOR('',#14898,1.);
#4211=VECTOR('',#14899,1.);
#4212=VECTOR('',#14900,1.);
#4213=VECTOR('',#14901,1.);
#4214=VECTOR('',#14904,1.);
#4215=VECTOR('',#14905,1.);
#4216=VECTOR('',#14906,1.);
#4217=VECTOR('',#14907,1.);
#4218=VECTOR('',#14910,1.);
#4219=VECTOR('',#14911,1.);
#4220=VECTOR('',#14912,1.);
#4221=VECTOR('',#14913,1.);
#4222=VECTOR('',#14914,1.);
#4223=VECTOR('',#14917,1.);
#4224=VECTOR('',#14918,1.);
#4225=VECTOR('',#14919,1.);
#4226=VECTOR('',#14920,1.);
#4227=VECTOR('',#14921,1.);
#4228=VECTOR('',#14952,0.225);
#4229=VECTOR('',#14959,0.225);
#4230=VECTOR('',#14964,1.);
#4231=VECTOR('',#14965,1.);
#4232=VECTOR('',#14966,1.);
#4233=VECTOR('',#14967,1.);
#4234=VECTOR('',#14970,1.);
#4235=VECTOR('',#14971,1.);
#4236=VECTOR('',#14972,1.);
#4237=VECTOR('',#14973,1.);
#4238=VECTOR('',#14976,1.);
#4239=VECTOR('',#14977,1.);
#4240=VECTOR('',#14978,1.);
#4241=VECTOR('',#14981,1.);
#4242=VECTOR('',#14982,1.);
#4243=VECTOR('',#14983,1.);
#4244=VECTOR('',#14986,1.);
#4245=VECTOR('',#14987,1.);
#4246=VECTOR('',#14988,1.);
#4247=VECTOR('',#14991,1.);
#4248=VECTOR('',#14992,1.);
#4249=VECTOR('',#14993,1.);
#4250=VECTOR('',#14998,1.);
#4251=VECTOR('',#14999,1.);
#4252=VECTOR('',#15000,1.);
#4253=VECTOR('',#15007,1.);
#4254=VECTOR('',#15008,1.);
#4255=VECTOR('',#15011,1.);
#4256=VECTOR('',#15012,1.);
#4257=VECTOR('',#15015,1.);
#4258=VECTOR('',#15022,1.);
#4259=VECTOR('',#15023,1.);
#4260=VECTOR('',#15024,1.);
#4261=VECTOR('',#15025,1.);
#4262=VECTOR('',#15028,1.);
#4263=VECTOR('',#15029,1.);
#4264=VECTOR('',#15030,1.);
#4265=VECTOR('',#15033,1.);
#4266=VECTOR('',#15034,1.);
#4267=VECTOR('',#15041,1.);
#4268=VECTOR('',#15042,1.);
#4269=VECTOR('',#15045,1.);
#4270=VECTOR('',#15054,1.);
#4271=VECTOR('',#15061,0.165);
#4272=VECTOR('',#15064,1.);
#4273=VECTOR('',#15067,0.5);
#4274=VECTOR('',#15072,0.605);
#4275=VECTOR('',#15075,1.4);
#4276=VECTOR('',#15086,0.165);
#4277=VECTOR('',#15093,0.165);
#4278=VECTOR('',#15100,0.165);
#4279=VECTOR('',#15107,0.165);
#4280=VECTOR('',#15114,0.225);
#4281=VECTOR('',#15121,0.225);
#4282=VECTOR('',#15128,1.6);
#4283=VECTOR('',#15133,1.);
#4284=VECTOR('',#15134,1.);
#4285=VECTOR('',#15135,1.);
#4286=VECTOR('',#15136,1.);
#4287=VECTOR('',#15139,1.);
#4288=VECTOR('',#15140,1.);
#4289=VECTOR('',#15141,1.);
#4290=VECTOR('',#15142,1.);
#4291=VECTOR('',#15145,1.);
#4292=VECTOR('',#15146,1.);
#4293=VECTOR('',#15147,1.);
#4294=VECTOR('',#15150,1.);
#4295=VECTOR('',#15151,1.);
#4296=VECTOR('',#15152,1.);
#4297=VECTOR('',#15155,1.);
#4298=VECTOR('',#15156,1.);
#4299=VECTOR('',#15157,1.);
#4300=VECTOR('',#15158,1.);
#4301=VECTOR('',#15161,1.);
#4302=VECTOR('',#15162,1.);
#4303=VECTOR('',#15165,1.);
#4304=VECTOR('',#15166,1.);
#4305=VECTOR('',#15167,1.);
#4306=VECTOR('',#15170,1.);
#4307=VECTOR('',#15181,0.225);
#4308=VECTOR('',#15188,0.225);
#4309=VECTOR('',#15195,0.225);
#4310=VECTOR('',#15202,0.225);
#4311=VECTOR('',#15209,1.59);
#4312=VECTOR('',#15218,1.41);
#4313=VECTOR('',#15225,2.4);
#4314=VECTOR('',#15238,0.225);
#4315=VECTOR('',#15245,0.225);
#4316=VECTOR('',#15252,0.225);
#4317=VECTOR('',#15259,0.225);
#4318=VECTOR('',#15266,1.59);
#4319=VECTOR('',#15277,1.41);
#4320=VECTOR('',#15282,2.4);
#4321=VECTOR('',#15295,0.165);
#4322=VECTOR('',#15302,0.165);
#4323=VECTOR('',#15309,0.165);
#4324=VECTOR('',#15316,0.165);
#4325=VECTOR('',#15323,0.225);
#4326=VECTOR('',#15330,0.225);
#4327=VECTOR('',#15337,1.6);
#4328=VECTOR('',#15342,1.);
#4329=VECTOR('',#15343,1.);
#4330=VECTOR('',#15344,1.);
#4331=VECTOR('',#15345,1.);
#4332=VECTOR('',#15348,1.);
#4333=VECTOR('',#15349,1.);
#4334=VECTOR('',#15350,1.);
#4335=VECTOR('',#15351,1.);
#4336=VECTOR('',#15354,1.);
#4337=VECTOR('',#15355,1.);
#4338=VECTOR('',#15356,1.);
#4339=VECTOR('',#15359,1.);
#4340=VECTOR('',#15360,1.);
#4341=VECTOR('',#15361,1.);
#4342=VECTOR('',#15364,1.);
#4343=VECTOR('',#15365,1.);
#4344=VECTOR('',#15366,1.);
#4345=VECTOR('',#15367,1.);
#4346=VECTOR('',#15370,1.);
#4347=VECTOR('',#15371,1.);
#4348=VECTOR('',#15374,1.);
#4349=VECTOR('',#15375,1.);
#4350=VECTOR('',#15376,1.);
#4351=VECTOR('',#15379,1.);
#4352=VECTOR('',#15390,0.225);
#4353=VECTOR('',#15397,0.225);
#4354=VECTOR('',#15404,0.225);
#4355=VECTOR('',#15411,0.225);
#4356=VECTOR('',#15418,1.59);
#4357=VECTOR('',#15427,1.41);
#4358=VECTOR('',#15434,2.4);
#4359=VECTOR('',#15447,0.225);
#4360=VECTOR('',#15454,0.225);
#4361=VECTOR('',#15461,0.225);
#4362=VECTOR('',#15468,0.225);
#4363=VECTOR('',#15475,1.59);
#4364=VECTOR('',#15486,1.41);
#4365=VECTOR('',#15491,2.4);
#4366=VECTOR('',#15508,0.55);
#4367=VECTOR('',#15513,0.6);
#4368=VECTOR('',#15534,1.070235);
#4369=VECTOR('',#15541,0.6);
#4370=VECTOR('',#15546,0.63);
#4371=VECTOR('',#15555,1.070235);
#4372=VECTOR('',#15562,0.63);
#4373=VECTOR('',#15581,1.129765);
#4374=VECTOR('',#15592,1.57);
#4375=VECTOR('',#15597,1.6);
#4376=VECTOR('',#15602,1.57);
#4377=VECTOR('',#15607,1.129765);
#4378=VECTOR('',#15654,1.123812);
#4379=VECTOR('',#15723,1.076188);
#4380=VECTOR('',#15752,1.119765);
#4381=VECTOR('',#15759,1.085235);
#4382=VECTOR('',#15770,1.119765);
#4383=VECTOR('',#15777,1.085235);
#4384=VECTOR('',#15792,1.);
#4385=VECTOR('',#15793,1.);
#4386=VECTOR('',#15794,1.);
#4387=VECTOR('',#15795,1.);
#4388=VECTOR('',#15798,1.);
#4389=VECTOR('',#15799,1.);
#4390=VECTOR('',#15800,1.);
#4391=VECTOR('',#15803,1.);
#4392=VECTOR('',#15804,1.);
#4393=VECTOR('',#15805,1.);
#4394=VECTOR('',#15808,1.);
#4395=VECTOR('',#15809,1.);
#4396=VECTOR('',#15810,1.);
#4397=VECTOR('',#15813,1.);
#4398=VECTOR('',#15814,1.);
#4399=VECTOR('',#15815,1.);
#4400=VECTOR('',#15818,1.);
#4401=VECTOR('',#15819,1.);
#4402=VECTOR('',#15836,0.325);
#4403=VECTOR('',#15841,0.35);
#4404=VECTOR('',#15846,0.335);
#4405=VECTOR('',#15855,0.21);
#4406=VECTOR('',#15858,0.2);
#4407=VECTOR('',#15867,0.425);
#4408=VECTOR('',#15874,1.);
#4409=VECTOR('',#15875,1.);
#4410=VECTOR('',#15876,1.);
#4411=VECTOR('',#15877,1.);
#4412=VECTOR('',#15880,1.);
#4413=VECTOR('',#15881,1.);
#4414=VECTOR('',#15882,1.);
#4415=VECTOR('',#15883,1.);
#4416=VECTOR('',#15888,1.);
#4417=VECTOR('',#15889,1.);
#4418=VECTOR('',#15890,1.);
#4419=VECTOR('',#15897,1.);
#4420=VECTOR('',#15898,1.);
#4421=VECTOR('',#15899,1.);
#4422=VECTOR('',#15904,1.);
#4423=VECTOR('',#15905,1.);
#4424=VECTOR('',#15906,1.);
#4425=VECTOR('',#15909,1.);
#4426=VECTOR('',#15910,1.);
#4427=VECTOR('',#15911,1.);
#4428=VECTOR('',#15914,1.);
#4429=VECTOR('',#15915,1.);
#4430=VECTOR('',#15916,1.);
#4431=VECTOR('',#15919,1.);
#4432=VECTOR('',#15920,1.);
#4433=VECTOR('',#15921,1.);
#4434=VECTOR('',#15924,1.);
#4435=VECTOR('',#15925,1.);
#4436=VECTOR('',#15926,1.);
#4437=VECTOR('',#15929,1.);
#4438=VECTOR('',#15930,1.);
#4439=VECTOR('',#15931,1.);
#4440=VECTOR('',#15934,1.);
#4441=VECTOR('',#15935,1.);
#4442=VECTOR('',#15936,1.);
#4443=VECTOR('',#15939,1.);
#4444=VECTOR('',#15940,1.);
#4445=VECTOR('',#15941,1.);
#4446=VECTOR('',#15944,1.);
#4447=VECTOR('',#15945,1.);
#4448=VECTOR('',#15946,1.);
#4449=VECTOR('',#15949,1.);
#4450=VECTOR('',#15950,1.);
#4451=VECTOR('',#15951,1.);
#4452=VECTOR('',#15954,1.);
#4453=VECTOR('',#15955,1.);
#4454=VECTOR('',#15956,1.);
#4455=VECTOR('',#15959,1.);
#4456=VECTOR('',#15960,1.);
#4457=VECTOR('',#15961,1.);
#4458=VECTOR('',#15964,1.);
#4459=VECTOR('',#15965,1.);
#4460=VECTOR('',#15966,1.);
#4461=VECTOR('',#15969,1.);
#4462=VECTOR('',#15970,1.);
#4463=VECTOR('',#15971,1.);
#4464=VECTOR('',#15974,1.);
#4465=VECTOR('',#15975,1.);
#4466=VECTOR('',#15976,1.);
#4467=VECTOR('',#15979,1.);
#4468=VECTOR('',#15980,1.);
#4469=VECTOR('',#15981,1.);
#4470=VECTOR('',#15984,1.);
#4471=VECTOR('',#15985,1.);
#4472=VECTOR('',#15986,1.);
#4473=VECTOR('',#15989,1.);
#4474=VECTOR('',#15990,1.);
#4475=VECTOR('',#15991,1.);
#4476=VECTOR('',#15994,1.);
#4477=VECTOR('',#15995,1.);
#4478=VECTOR('',#15996,1.);
#4479=VECTOR('',#15999,1.);
#4480=VECTOR('',#16000,1.);
#4481=VECTOR('',#16001,1.);
#4482=VECTOR('',#16004,1.);
#4483=VECTOR('',#16005,1.);
#4484=VECTOR('',#16006,1.);
#4485=VECTOR('',#16009,1.);
#4486=VECTOR('',#16010,1.);
#4487=VECTOR('',#16011,1.);
#4488=VECTOR('',#16014,1.);
#4489=VECTOR('',#16015,1.);
#4490=VECTOR('',#16016,1.);
#4491=VECTOR('',#16019,1.);
#4492=VECTOR('',#16020,1.);
#4493=VECTOR('',#16021,1.);
#4494=VECTOR('',#16024,1.);
#4495=VECTOR('',#16025,1.);
#4496=VECTOR('',#16026,1.);
#4497=VECTOR('',#16029,1.);
#4498=VECTOR('',#16030,1.);
#4499=VECTOR('',#16031,1.);
#4500=VECTOR('',#16034,1.);
#4501=VECTOR('',#16035,1.);
#4502=VECTOR('',#16036,1.);
#4503=VECTOR('',#16039,1.);
#4504=VECTOR('',#16040,1.);
#4505=VECTOR('',#16041,1.);
#4506=VECTOR('',#16044,1.);
#4507=VECTOR('',#16045,1.);
#4508=VECTOR('',#16046,1.);
#4509=VECTOR('',#16049,1.);
#4510=VECTOR('',#16050,1.);
#4511=VECTOR('',#16051,1.);
#4512=VECTOR('',#16054,1.);
#4513=VECTOR('',#16055,1.);
#4514=VECTOR('',#16056,1.);
#4515=VECTOR('',#16059,1.);
#4516=VECTOR('',#16060,1.);
#4517=VECTOR('',#16061,1.);
#4518=VECTOR('',#16064,1.);
#4519=VECTOR('',#16065,1.);
#4520=VECTOR('',#16066,1.);
#4521=VECTOR('',#16069,1.);
#4522=VECTOR('',#16070,1.);
#4523=VECTOR('',#16071,1.);
#4524=VECTOR('',#16074,1.);
#4525=VECTOR('',#16075,1.);
#4526=VECTOR('',#16076,1.);
#4527=VECTOR('',#16079,1.);
#4528=VECTOR('',#16080,1.);
#4529=VECTOR('',#16081,1.);
#4530=VECTOR('',#16084,1.);
#4531=VECTOR('',#16085,1.);
#4532=VECTOR('',#16086,1.);
#4533=VECTOR('',#16089,1.);
#4534=VECTOR('',#16090,1.);
#4535=VECTOR('',#16091,1.);
#4536=VECTOR('',#16094,1.);
#4537=VECTOR('',#16095,1.);
#4538=VECTOR('',#16096,1.);
#4539=VECTOR('',#16099,1.);
#4540=VECTOR('',#16100,1.);
#4541=VECTOR('',#16101,1.);
#4542=VECTOR('',#16104,1.);
#4543=VECTOR('',#16105,1.);
#4544=VECTOR('',#16106,1.);
#4545=VECTOR('',#16109,1.);
#4546=VECTOR('',#16110,1.);
#4547=VECTOR('',#16111,1.);
#4548=VECTOR('',#16114,1.);
#4549=VECTOR('',#16115,1.);
#4550=VECTOR('',#16116,1.);
#4551=VECTOR('',#16119,1.);
#4552=VECTOR('',#16120,1.);
#4553=VECTOR('',#16121,1.);
#4554=VECTOR('',#16124,1.);
#4555=VECTOR('',#16125,1.);
#4556=VECTOR('',#16126,1.);
#4557=VECTOR('',#16129,1.);
#4558=VECTOR('',#16130,1.);
#4559=VECTOR('',#16131,1.);
#4560=VECTOR('',#16134,1.);
#4561=VECTOR('',#16135,1.);
#4562=VECTOR('',#16136,1.);
#4563=VECTOR('',#16139,1.);
#4564=VECTOR('',#16140,1.);
#4565=VECTOR('',#16141,1.);
#4566=VECTOR('',#16144,1.);
#4567=VECTOR('',#16145,1.);
#4568=VECTOR('',#16146,1.);
#4569=VECTOR('',#16149,1.);
#4570=VECTOR('',#16150,1.);
#4571=VECTOR('',#16151,1.);
#4572=VECTOR('',#16154,1.);
#4573=VECTOR('',#16155,1.);
#4574=VECTOR('',#16156,1.);
#4575=VECTOR('',#16159,1.);
#4576=VECTOR('',#16160,1.);
#4577=VECTOR('',#16161,1.);
#4578=VECTOR('',#16164,1.);
#4579=VECTOR('',#16165,1.);
#4580=VECTOR('',#16166,1.);
#4581=VECTOR('',#16169,1.);
#4582=VECTOR('',#16170,1.);
#4583=VECTOR('',#16171,1.);
#4584=VECTOR('',#16174,1.);
#4585=VECTOR('',#16175,1.);
#4586=VECTOR('',#16176,1.);
#4587=VECTOR('',#16179,1.);
#4588=VECTOR('',#16180,1.);
#4589=VECTOR('',#16181,1.);
#4590=VECTOR('',#16184,1.);
#4591=VECTOR('',#16185,1.);
#4592=VECTOR('',#16186,1.);
#4593=VECTOR('',#16189,1.);
#4594=VECTOR('',#16190,1.);
#4595=VECTOR('',#16191,1.);
#4596=VECTOR('',#16194,1.);
#4597=VECTOR('',#16195,1.);
#4598=VECTOR('',#16196,1.);
#4599=VECTOR('',#16199,1.);
#4600=VECTOR('',#16200,1.);
#4601=VECTOR('',#16201,1.);
#4602=VECTOR('',#16204,1.);
#4603=VECTOR('',#16205,1.);
#4604=VECTOR('',#16206,1.);
#4605=VECTOR('',#16209,1.);
#4606=VECTOR('',#16210,1.);
#4607=VECTOR('',#16211,1.);
#4608=VECTOR('',#16214,1.);
#4609=VECTOR('',#16215,1.);
#4610=VECTOR('',#16216,1.);
#4611=VECTOR('',#16219,1.);
#4612=VECTOR('',#16220,1.);
#4613=VECTOR('',#16221,1.);
#4614=VECTOR('',#16224,1.);
#4615=VECTOR('',#16225,1.);
#4616=VECTOR('',#16226,1.);
#4617=VECTOR('',#16229,1.);
#4618=VECTOR('',#16230,1.);
#4619=VECTOR('',#16231,1.);
#4620=VECTOR('',#16234,1.);
#4621=VECTOR('',#16235,1.);
#4622=VECTOR('',#16236,1.);
#4623=VECTOR('',#16239,1.);
#4624=VECTOR('',#16240,1.);
#4625=VECTOR('',#16241,1.);
#4626=VECTOR('',#16244,1.);
#4627=VECTOR('',#16245,1.);
#4628=VECTOR('',#16246,1.);
#4629=VECTOR('',#16249,1.);
#4630=VECTOR('',#16250,1.);
#4631=VECTOR('',#16251,1.);
#4632=VECTOR('',#16254,1.);
#4633=VECTOR('',#16255,1.);
#4634=VECTOR('',#16256,1.);
#4635=VECTOR('',#16259,1.);
#4636=VECTOR('',#16260,1.);
#4637=VECTOR('',#16261,1.);
#4638=VECTOR('',#16264,1.);
#4639=VECTOR('',#16265,1.);
#4640=VECTOR('',#16266,1.);
#4641=VECTOR('',#16269,1.);
#4642=VECTOR('',#16270,1.);
#4643=VECTOR('',#16271,1.);
#4644=VECTOR('',#16274,1.);
#4645=VECTOR('',#16275,1.);
#4646=VECTOR('',#16276,1.);
#4647=VECTOR('',#16279,1.);
#4648=VECTOR('',#16280,1.);
#4649=VECTOR('',#16281,1.);
#4650=VECTOR('',#16284,1.);
#4651=VECTOR('',#16285,1.);
#4652=VECTOR('',#16286,1.);
#4653=VECTOR('',#16289,1.);
#4654=VECTOR('',#16290,1.);
#4655=VECTOR('',#16291,1.);
#4656=VECTOR('',#16294,1.);
#4657=VECTOR('',#16295,1.);
#4658=VECTOR('',#16296,1.);
#4659=VECTOR('',#16299,1.);
#4660=VECTOR('',#16300,1.);
#4661=VECTOR('',#16301,1.);
#4662=VECTOR('',#16304,1.);
#4663=VECTOR('',#16305,1.);
#4664=VECTOR('',#16306,1.);
#4665=VECTOR('',#16309,1.);
#4666=VECTOR('',#16310,1.);
#4667=VECTOR('',#16311,1.);
#4668=VECTOR('',#16314,1.);
#4669=VECTOR('',#16315,1.);
#4670=VECTOR('',#16316,1.);
#4671=VECTOR('',#16319,1.);
#4672=VECTOR('',#16320,1.);
#4673=VECTOR('',#16321,1.);
#4674=VECTOR('',#16324,1.);
#4675=VECTOR('',#16325,1.);
#4676=VECTOR('',#16326,1.);
#4677=VECTOR('',#16329,1.);
#4678=VECTOR('',#16330,1.);
#4679=VECTOR('',#16331,1.);
#4680=VECTOR('',#16334,1.);
#4681=VECTOR('',#16335,1.);
#4682=VECTOR('',#16336,1.);
#4683=VECTOR('',#16339,1.);
#4684=VECTOR('',#16340,1.);
#4685=VECTOR('',#16341,1.);
#4686=VECTOR('',#16344,1.);
#4687=VECTOR('',#16345,1.);
#4688=VECTOR('',#16346,1.);
#4689=VECTOR('',#16349,1.);
#4690=VECTOR('',#16350,1.);
#4691=VECTOR('',#16351,1.);
#4692=VECTOR('',#16354,1.);
#4693=VECTOR('',#16355,1.);
#4694=VECTOR('',#16356,1.);
#4695=VECTOR('',#16359,1.);
#4696=VECTOR('',#16360,1.);
#4697=VECTOR('',#16361,1.);
#4698=VECTOR('',#16364,1.);
#4699=VECTOR('',#16365,1.);
#4700=VECTOR('',#16366,1.);
#4701=VECTOR('',#16369,1.);
#4702=VECTOR('',#16370,1.);
#4703=VECTOR('',#16371,1.);
#4704=VECTOR('',#16374,1.);
#4705=VECTOR('',#16375,1.);
#4706=VECTOR('',#16376,1.);
#4707=VECTOR('',#16379,1.);
#4708=VECTOR('',#16380,1.);
#4709=VECTOR('',#16381,1.);
#4710=VECTOR('',#16384,1.);
#4711=VECTOR('',#16385,1.);
#4712=VECTOR('',#16386,1.);
#4713=VECTOR('',#16389,1.);
#4714=VECTOR('',#16390,1.);
#4715=VECTOR('',#16391,1.);
#4716=VECTOR('',#16394,1.);
#4717=VECTOR('',#16395,1.);
#4718=VECTOR('',#16396,1.);
#4719=VECTOR('',#16399,1.);
#4720=VECTOR('',#16400,1.);
#4721=VECTOR('',#16401,1.);
#4722=VECTOR('',#16404,1.);
#4723=VECTOR('',#16405,1.);
#4724=VECTOR('',#16406,1.);
#4725=VECTOR('',#16409,1.);
#4726=VECTOR('',#16410,1.);
#4727=VECTOR('',#16411,1.);
#4728=VECTOR('',#16414,1.);
#4729=VECTOR('',#16415,1.);
#4730=VECTOR('',#16416,1.);
#4731=VECTOR('',#16419,1.);
#4732=VECTOR('',#16420,1.);
#4733=VECTOR('',#16421,1.);
#4734=VECTOR('',#16424,1.);
#4735=VECTOR('',#16425,1.);
#4736=VECTOR('',#16426,1.);
#4737=VECTOR('',#16429,1.);
#4738=VECTOR('',#16430,1.);
#4739=VECTOR('',#16431,1.);
#4740=VECTOR('',#16434,1.);
#4741=VECTOR('',#16435,1.);
#4742=VECTOR('',#16436,1.);
#4743=VECTOR('',#16439,1.);
#4744=VECTOR('',#16440,1.);
#4745=VECTOR('',#16441,1.);
#4746=VECTOR('',#16444,1.);
#4747=VECTOR('',#16445,1.);
#4748=VECTOR('',#16446,1.);
#4749=VECTOR('',#16449,1.);
#4750=VECTOR('',#16450,1.);
#4751=VECTOR('',#16451,1.);
#4752=VECTOR('',#16454,1.);
#4753=VECTOR('',#16455,1.);
#4754=VECTOR('',#16456,1.);
#4755=VECTOR('',#16459,1.);
#4756=VECTOR('',#16460,1.);
#4757=VECTOR('',#16461,1.);
#4758=VECTOR('',#16464,1.);
#4759=VECTOR('',#16465,1.);
#4760=VECTOR('',#16466,1.);
#4761=VECTOR('',#16469,1.);
#4762=VECTOR('',#16470,1.);
#4763=VECTOR('',#16471,1.);
#4764=VECTOR('',#16474,1.);
#4765=VECTOR('',#16475,1.);
#4766=VECTOR('',#16476,1.);
#4767=VECTOR('',#16479,1.);
#4768=VECTOR('',#16480,1.);
#4769=VECTOR('',#16481,1.);
#4770=VECTOR('',#16484,1.);
#4771=VECTOR('',#16485,1.);
#4772=VECTOR('',#16486,1.);
#4773=VECTOR('',#16489,1.);
#4774=VECTOR('',#16490,1.);
#4775=VECTOR('',#16491,1.);
#4776=VECTOR('',#16494,1.);
#4777=VECTOR('',#16495,1.);
#4778=VECTOR('',#16496,1.);
#4779=VECTOR('',#16499,1.);
#4780=VECTOR('',#16500,1.);
#4781=VECTOR('',#16501,1.);
#4782=VECTOR('',#16504,1.);
#4783=VECTOR('',#16505,1.);
#4784=VECTOR('',#16506,1.);
#4785=VECTOR('',#16509,1.);
#4786=VECTOR('',#16510,1.);
#4787=VECTOR('',#16511,1.);
#4788=VECTOR('',#16514,1.);
#4789=VECTOR('',#16515,1.);
#4790=VECTOR('',#16516,1.);
#4791=VECTOR('',#16519,1.);
#4792=VECTOR('',#16520,1.);
#4793=VECTOR('',#16521,1.);
#4794=VECTOR('',#16524,1.);
#4795=VECTOR('',#16525,1.);
#4796=VECTOR('',#16526,1.);
#4797=VECTOR('',#16529,1.);
#4798=VECTOR('',#16530,1.);
#4799=VECTOR('',#16531,1.);
#4800=VECTOR('',#16534,1.);
#4801=VECTOR('',#16535,1.);
#4802=VECTOR('',#16536,1.);
#4803=VECTOR('',#16539,1.);
#4804=VECTOR('',#16540,1.);
#4805=VECTOR('',#16541,1.);
#4806=VECTOR('',#16544,1.);
#4807=VECTOR('',#16545,1.);
#4808=VECTOR('',#16546,1.);
#4809=VECTOR('',#16549,1.);
#4810=VECTOR('',#16550,1.);
#4811=VECTOR('',#16551,1.);
#4812=VECTOR('',#16554,1.);
#4813=VECTOR('',#16555,1.);
#4814=VECTOR('',#16556,1.);
#4815=VECTOR('',#16559,1.);
#4816=VECTOR('',#16560,1.);
#4817=VECTOR('',#16561,1.);
#4818=VECTOR('',#16564,1.);
#4819=VECTOR('',#16565,1.);
#4820=VECTOR('',#16566,1.);
#4821=VECTOR('',#16569,1.);
#4822=VECTOR('',#16570,1.);
#4823=VECTOR('',#16571,1.);
#4824=VECTOR('',#16574,1.);
#4825=VECTOR('',#16575,1.);
#4826=VECTOR('',#16576,1.);
#4827=VECTOR('',#16579,1.);
#4828=VECTOR('',#16580,1.);
#4829=VECTOR('',#16581,1.);
#4830=VECTOR('',#16584,1.);
#4831=VECTOR('',#16585,1.);
#4832=VECTOR('',#16586,1.);
#4833=VECTOR('',#16589,1.);
#4834=VECTOR('',#16590,1.);
#4835=VECTOR('',#16591,1.);
#4836=VECTOR('',#16594,1.);
#4837=VECTOR('',#16595,1.);
#4838=VECTOR('',#16596,1.);
#4839=VECTOR('',#16599,1.);
#4840=VECTOR('',#16600,1.);
#4841=VECTOR('',#16601,1.);
#4842=VECTOR('',#16604,1.);
#4843=VECTOR('',#16605,1.);
#4844=VECTOR('',#16606,1.);
#4845=VECTOR('',#16609,1.);
#4846=VECTOR('',#16610,1.);
#4847=VECTOR('',#16611,1.);
#4848=VECTOR('',#16614,1.);
#4849=VECTOR('',#16615,1.);
#4850=VECTOR('',#16616,1.);
#4851=VECTOR('',#16619,1.);
#4852=VECTOR('',#16620,1.);
#4853=VECTOR('',#16621,1.);
#4854=VECTOR('',#16624,1.);
#4855=VECTOR('',#16625,1.);
#4856=VECTOR('',#16626,1.);
#4857=VECTOR('',#16629,1.);
#4858=VECTOR('',#16630,1.);
#4859=VECTOR('',#16631,1.);
#4860=VECTOR('',#16634,1.);
#4861=VECTOR('',#16635,1.);
#4862=VECTOR('',#16636,1.);
#4863=VECTOR('',#16639,1.);
#4864=VECTOR('',#16640,1.);
#4865=VECTOR('',#16641,1.);
#4866=VECTOR('',#16644,1.);
#4867=VECTOR('',#16645,1.);
#4868=VECTOR('',#16646,1.);
#4869=VECTOR('',#16649,1.);
#4870=VECTOR('',#16650,1.);
#4871=VECTOR('',#16651,1.);
#4872=VECTOR('',#16654,1.);
#4873=VECTOR('',#16655,1.);
#4874=VECTOR('',#16656,1.);
#4875=VECTOR('',#16659,1.);
#4876=VECTOR('',#16660,1.);
#4877=VECTOR('',#16661,1.);
#4878=VECTOR('',#16664,1.);
#4879=VECTOR('',#16665,1.);
#4880=VECTOR('',#16666,1.);
#4881=VECTOR('',#16669,1.);
#4882=VECTOR('',#16670,1.);
#4883=VECTOR('',#16671,1.);
#4884=VECTOR('',#16674,1.);
#4885=VECTOR('',#16675,1.);
#4886=VECTOR('',#16676,1.);
#4887=VECTOR('',#16679,1.);
#4888=VECTOR('',#16680,1.);
#4889=VECTOR('',#16681,1.);
#4890=VECTOR('',#16684,1.);
#4891=VECTOR('',#16685,1.);
#4892=VECTOR('',#16686,1.);
#4893=VECTOR('',#16689,1.);
#4894=VECTOR('',#16690,1.);
#4895=VECTOR('',#16691,1.);
#4896=VECTOR('',#16694,1.);
#4897=VECTOR('',#16695,1.);
#4898=VECTOR('',#16696,1.);
#4899=VECTOR('',#16699,1.);
#4900=VECTOR('',#16700,1.);
#4901=VECTOR('',#16701,1.);
#4902=VECTOR('',#16704,1.);
#4903=VECTOR('',#16705,1.);
#4904=VECTOR('',#16714,1.);
#4905=VECTOR('',#16715,1.);
#4906=VECTOR('',#16726,1.);
#4907=VECTOR('',#16733,0.164999999999999);
#4908=VECTOR('',#16736,1.);
#4909=VECTOR('',#16741,0.3);
#4910=VECTOR('',#16748,0.5);
#4911=VECTOR('',#16757,1.4);
#4912=VECTOR('',#16770,0.3);
#4913=VECTOR('',#16783,0.199999999999999);
#4914=VECTOR('',#16794,0.164999999999999);
#4915=VECTOR('',#16797,1.);
#4916=VECTOR('',#16798,1.);
#4917=VECTOR('',#16799,1.);
#4918=VECTOR('',#16800,1.);
#4919=VECTOR('',#16803,1.);
#4920=VECTOR('',#16804,1.);
#4921=VECTOR('',#16805,1.);
#4922=VECTOR('',#16806,1.);
#4923=VECTOR('',#16809,1.);
#4924=VECTOR('',#16810,1.);
#4925=VECTOR('',#16811,1.);
#4926=VECTOR('',#16814,1.);
#4927=VECTOR('',#16815,1.);
#4928=VECTOR('',#16816,1.);
#4929=VECTOR('',#16837,1.);
#4930=VECTOR('',#16838,1.);
#4931=VECTOR('',#16839,1.);
#4932=VECTOR('',#16840,1.);
#4933=VECTOR('',#16843,1.);
#4934=VECTOR('',#16844,1.);
#4935=VECTOR('',#16845,1.);
#4936=VECTOR('',#16848,1.);
#4937=VECTOR('',#16849,1.);
#4938=VECTOR('',#16850,1.);
#4939=VECTOR('',#16853,1.);
#4940=VECTOR('',#16854,1.);
#4941=VECTOR('',#16855,1.);
#4942=VECTOR('',#16858,1.);
#4943=VECTOR('',#16859,1.);
#4944=VECTOR('',#16860,1.);
#4945=VECTOR('',#16863,1.);
#4946=VECTOR('',#16864,1.);
#4947=VECTOR('',#16875,0.185);
#4948=VECTOR('',#16880,0.2);
#4949=VECTOR('',#16885,0.1625);
#4950=VECTOR('',#16908,0.165);
#4951=VECTOR('',#16917,0.165);
#4952=VECTOR('',#16924,1.);
#4953=VECTOR('',#16925,1.);
#4954=VECTOR('',#16926,1.);
#4955=VECTOR('',#16927,1.);
#4956=VECTOR('',#16932,1.);
#4957=VECTOR('',#16933,1.);
#4958=VECTOR('',#16936,1.);
#4959=VECTOR('',#16937,1.);
#4960=VECTOR('',#16940,1.);
#4961=VECTOR('',#16941,1.);
#4962=VECTOR('',#16948,1.);
#4963=VECTOR('',#16949,1.);
#4964=VECTOR('',#16950,1.);
#4965=VECTOR('',#16951,1.);
#4966=VECTOR('',#16956,1.);
#4967=VECTOR('',#16957,1.);
#4968=VECTOR('',#16960,1.);
#4969=VECTOR('',#16961,1.);
#4970=VECTOR('',#16964,1.);
#4971=VECTOR('',#16965,1.);
#4972=VECTOR('',#16974,0.6);
#4973=VECTOR('',#16987,0.605);
#4974=VECTOR('',#16994,0.8);
#4975=VECTOR('',#17007,0.605);
#4976=VECTOR('',#17014,0.8);
#4977=VECTOR('',#17027,0.605);
#4978=VECTOR('',#17034,0.8);
#4979=VECTOR('',#17047,0.605);
#4980=VECTOR('',#17054,0.8);
#4981=VECTOR('',#17065,1.);
#4982=VECTOR('',#17066,1.);
#4983=VECTOR('',#17067,1.);
#4984=VECTOR('',#17068,1.);
#4985=VECTOR('',#17071,1.);
#4986=VECTOR('',#17072,1.);
#4987=VECTOR('',#17073,1.);
#4988=VECTOR('',#17076,1.);
#4989=VECTOR('',#17077,1.);
#4990=VECTOR('',#17078,1.);
#4991=VECTOR('',#17081,1.);
#4992=VECTOR('',#17082,1.);
#4993=VECTOR('',#17091,1.);
#4994=VECTOR('',#17092,1.);
#4995=VECTOR('',#17093,1.);
#4996=VECTOR('',#17094,1.);
#4997=VECTOR('',#17097,1.);
#4998=VECTOR('',#17098,1.);
#4999=VECTOR('',#17099,1.);
#5000=VECTOR('',#17102,1.);
#5001=VECTOR('',#17103,1.);
#5002=VECTOR('',#17104,1.);
#5003=VECTOR('',#17107,1.);
#5004=VECTOR('',#17108,1.);
#5005=VECTOR('',#17119,0.25);
#5006=VECTOR('',#17124,1.);
#5007=VECTOR('',#17125,1.);
#5008=VECTOR('',#17126,1.);
#5009=VECTOR('',#17127,1.);
#5010=VECTOR('',#17130,1.);
#5011=VECTOR('',#17131,1.);
#5012=VECTOR('',#17132,1.);
#5013=VECTOR('',#17135,1.);
#5014=VECTOR('',#17136,1.);
#5015=VECTOR('',#17137,1.);
#5016=VECTOR('',#17150,1.);
#5017=VECTOR('',#17153,1.);
#5018=VECTOR('',#17158,1.);
#5019=VECTOR('',#17159,1.);
#5020=VECTOR('',#17160,1.);
#5021=VECTOR('',#17163,1.);
#5022=VECTOR('',#17168,1.);
#5023=VECTOR('',#17169,1.);
#5024=VECTOR('',#17176,1.3);
#5025=VECTOR('',#17187,0.33);
#5026=VECTOR('',#17194,0.4);
#5027=VECTOR('',#17207,0.225);
#5028=VECTOR('',#17214,1.);
#5029=VECTOR('',#17227,0.225);
#5030=VECTOR('',#17234,1.);
#5031=VECTOR('',#17245,1.);
#5032=VECTOR('',#17246,1.);
#5033=VECTOR('',#17247,1.);
#5034=VECTOR('',#17248,1.);
#5035=VECTOR('',#17251,1.);
#5036=VECTOR('',#17252,1.);
#5037=VECTOR('',#17253,1.);
#5038=VECTOR('',#17256,1.);
#5039=VECTOR('',#17257,1.);
#5040=VECTOR('',#17258,1.);
#5041=VECTOR('',#17263,1.);
#5042=VECTOR('',#17266,1.);
#5043=VECTOR('',#17269,1.);
#5044=VECTOR('',#17272,1.);
#5045=VECTOR('',#17275,1.);
#5046=VECTOR('',#17278,1.);
#5047=VECTOR('',#17281,1.);
#5048=VECTOR('',#17284,1.);
#5049=VECTOR('',#17287,1.);
#5050=VECTOR('',#17290,1.);
#5051=VECTOR('',#17293,1.);
#5052=VECTOR('',#17296,1.);
#5053=VECTOR('',#17299,1.);
#5054=VECTOR('',#17302,1.);
#5055=VECTOR('',#17305,1.);
#5056=VECTOR('',#17308,1.);
#5057=VECTOR('',#17311,1.);
#5058=VECTOR('',#17314,1.);
#5059=VECTOR('',#17317,1.);
#5060=VECTOR('',#17320,1.);
#5061=VECTOR('',#17331,1.4);
#5062=VECTOR('',#17336,1.);
#5063=VECTOR('',#17337,1.);
#5064=VECTOR('',#17340,1.);
#5065=VECTOR('',#17341,1.);
#5066=VECTOR('',#17342,1.);
#5067=VECTOR('',#17347,1.);
#5068=VECTOR('',#17348,1.);
#5069=VECTOR('',#17351,1.);
#5070=VECTOR('',#17352,1.);
#5071=VECTOR('',#17353,1.);
#5072=VECTOR('',#17358,1.);
#5073=VECTOR('',#17359,1.);
#5074=VECTOR('',#17362,1.);
#5075=VECTOR('',#17363,1.);
#5076=VECTOR('',#17364,1.);
#5077=VECTOR('',#17369,1.);
#5078=VECTOR('',#17370,1.);
#5079=VECTOR('',#17373,1.);
#5080=VECTOR('',#17374,1.);
#5081=VECTOR('',#17375,1.);
#5082=VECTOR('',#17380,1.);
#5083=VECTOR('',#17381,1.);
#5084=VECTOR('',#17384,1.);
#5085=VECTOR('',#17385,1.);
#5086=VECTOR('',#17386,1.);
#5087=VECTOR('',#17391,1.);
#5088=VECTOR('',#17392,1.);
#5089=VECTOR('',#17395,1.);
#5090=VECTOR('',#17396,1.);
#5091=VECTOR('',#17397,1.);
#5092=VECTOR('',#17402,1.);
#5093=VECTOR('',#17403,1.);
#5094=VECTOR('',#17406,1.);
#5095=VECTOR('',#17407,1.);
#5096=VECTOR('',#17408,1.);
#5097=VECTOR('',#17413,1.);
#5098=VECTOR('',#17414,1.);
#5099=VECTOR('',#17417,1.);
#5100=VECTOR('',#17418,1.);
#5101=VECTOR('',#17419,1.);
#5102=VECTOR('',#17424,1.);
#5103=VECTOR('',#17425,1.);
#5104=VECTOR('',#17428,1.);
#5105=VECTOR('',#17429,1.);
#5106=VECTOR('',#17430,1.);
#5107=VECTOR('',#17435,1.);
#5108=VECTOR('',#17436,1.);
#5109=VECTOR('',#17439,1.);
#5110=VECTOR('',#17440,1.);
#5111=VECTOR('',#17441,1.);
#5112=VECTOR('',#17446,1.);
#5113=VECTOR('',#17447,1.);
#5114=VECTOR('',#17450,1.);
#5115=VECTOR('',#17451,1.);
#5116=VECTOR('',#17452,1.);
#5117=VECTOR('',#17457,1.);
#5118=VECTOR('',#17458,1.);
#5119=VECTOR('',#17461,1.);
#5120=VECTOR('',#17462,1.);
#5121=VECTOR('',#17463,1.);
#5122=VECTOR('',#17468,1.);
#5123=VECTOR('',#17469,1.);
#5124=VECTOR('',#17472,1.);
#5125=VECTOR('',#17473,1.);
#5126=VECTOR('',#17474,1.);
#5127=VECTOR('',#17479,1.);
#5128=VECTOR('',#17480,1.);
#5129=VECTOR('',#17483,1.);
#5130=VECTOR('',#17484,1.);
#5131=VECTOR('',#17485,1.);
#5132=VECTOR('',#17490,1.);
#5133=VECTOR('',#17491,1.);
#5134=VECTOR('',#17494,1.);
#5135=VECTOR('',#17495,1.);
#5136=VECTOR('',#17496,1.);
#5137=VECTOR('',#17501,1.);
#5138=VECTOR('',#17502,1.);
#5139=VECTOR('',#17505,1.);
#5140=VECTOR('',#17506,1.);
#5141=VECTOR('',#17507,1.);
#5142=VECTOR('',#17512,1.);
#5143=VECTOR('',#17513,1.);
#5144=VECTOR('',#17516,1.);
#5145=VECTOR('',#17517,1.);
#5146=VECTOR('',#17518,1.);
#5147=VECTOR('',#17523,1.);
#5148=VECTOR('',#17524,1.);
#5149=VECTOR('',#17527,1.);
#5150=VECTOR('',#17528,1.);
#5151=VECTOR('',#17529,1.);
#5152=VECTOR('',#17534,1.);
#5153=VECTOR('',#17535,1.);
#5154=VECTOR('',#17538,1.);
#5155=VECTOR('',#17539,1.);
#5156=VECTOR('',#17540,1.);
#5157=VECTOR('',#17545,1.);
#5158=VECTOR('',#17546,1.);
#5159=VECTOR('',#17549,1.);
#5160=VECTOR('',#17550,1.);
#5161=VECTOR('',#17551,1.);
#5162=VECTOR('',#17564,0.32);
#5163=VECTOR('',#17571,0.6);
#5164=VECTOR('',#17588,0.475);
#5165=VECTOR('',#17593,0.5);
#5166=VECTOR('',#17598,0.485);
#5167=VECTOR('',#17607,0.31);
#5168=VECTOR('',#17612,0.3);
#5169=VECTOR('',#17617,0.27);
#5170=VECTOR('',#17622,1.);
#5171=VECTOR('',#17623,1.);
#5172=VECTOR('',#17624,1.);
#5173=VECTOR('',#17625,1.);
#5174=VECTOR('',#17628,1.);
#5175=VECTOR('',#17629,1.);
#5176=VECTOR('',#17630,1.);
#5177=VECTOR('',#17633,1.);
#5178=VECTOR('',#17634,1.);
#5179=VECTOR('',#17635,1.);
#5180=VECTOR('',#17638,1.);
#5181=VECTOR('',#17639,1.);
#5182=VECTOR('',#17640,1.);
#5183=VECTOR('',#17643,1.);
#5184=VECTOR('',#17644,1.);
#5185=VECTOR('',#17645,1.);
#5186=VECTOR('',#17648,1.);
#5187=VECTOR('',#17649,1.);
#5188=VECTOR('',#17664,0.325);
#5189=VECTOR('',#17669,0.35);
#5190=VECTOR('',#17674,0.335);
#5191=VECTOR('',#17683,0.21);
#5192=VECTOR('',#17688,0.2);
#5193=VECTOR('',#17693,0.18);
#5194=VECTOR('',#17698,1.);
#5195=VECTOR('',#17699,1.);
#5196=VECTOR('',#17700,1.);
#5197=VECTOR('',#17701,1.);
#5198=VECTOR('',#17704,1.);
#5199=VECTOR('',#17705,1.);
#5200=VECTOR('',#17706,1.);
#5201=VECTOR('',#17709,1.);
#5202=VECTOR('',#17710,1.);
#5203=VECTOR('',#17711,1.);
#5204=VECTOR('',#17714,1.);
#5205=VECTOR('',#17715,1.);
#5206=VECTOR('',#17716,1.);
#5207=VECTOR('',#17719,1.);
#5208=VECTOR('',#17720,1.);
#5209=VECTOR('',#17721,1.);
#5210=VECTOR('',#17724,1.);
#5211=VECTOR('',#17725,1.);
#5212=VECTOR('',#17866,0.405);
#5213=VECTOR('',#17873,0.9);
#5214=CIRCLE('',#13192,0.165);
#5215=CIRCLE('',#13193,0.165);
#5216=CIRCLE('',#13195,0.165);
#5217=CIRCLE('',#13196,0.165);
#5218=CIRCLE('',#13198,0.165);
#5219=CIRCLE('',#13199,0.165);
#5220=CIRCLE('',#13201,0.165);
#5221=CIRCLE('',#13202,0.165);
#5222=CIRCLE('',#13204,0.165);
#5223=CIRCLE('',#13205,0.165);
#5224=CIRCLE('',#13207,0.165);
#5225=CIRCLE('',#13208,0.165);
#5226=CIRCLE('',#13231,0.165);
#5227=CIRCLE('',#13232,0.165);
#5228=CIRCLE('',#13235,0.165);
#5229=CIRCLE('',#13236,0.165);
#5230=CIRCLE('',#13241,2.);
#5231=CIRCLE('',#13242,2.);
#5232=CIRCLE('',#13243,1.4);
#5233=CIRCLE('',#13245,1.4);
#5234=CIRCLE('',#13247,2.);
#5235=CIRCLE('',#13249,2.);
#5236=CIRCLE('',#13254,0.165);
#5237=CIRCLE('',#13255,0.165);
#5238=CIRCLE('',#13258,0.165);
#5239=CIRCLE('',#13259,0.165);
#5240=CIRCLE('',#13264,2.);
#5241=CIRCLE('',#13265,1.4);
#5242=CIRCLE('',#13266,1.4);
#5243=CIRCLE('',#13267,2.);
#5244=CIRCLE('',#13268,1.4);
#5245=CIRCLE('',#13270,1.4);
#5246=CIRCLE('',#13272,2.);
#5247=CIRCLE('',#13274,2.);
#5248=CIRCLE('',#13280,0.164999999999999);
#5249=CIRCLE('',#13282,0.164999999999999);
#5250=CIRCLE('',#13285,1.4);
#5251=CIRCLE('',#13287,0.605);
#5252=CIRCLE('',#13288,0.605);
#5253=CIRCLE('',#13290,1.4);
#5254=CIRCLE('',#13299,0.375);
#5255=CIRCLE('',#13300,0.375);
#5256=CIRCLE('',#13302,1.4);
#5257=CIRCLE('',#13304,0.375);
#5258=CIRCLE('',#13305,0.375);
#5259=CIRCLE('',#13307,1.4);
#5260=CIRCLE('',#13309,2.);
#5261=CIRCLE('',#13310,1.4);
#5262=CIRCLE('',#13311,1.4);
#5263=CIRCLE('',#13312,1.4);
#5264=CIRCLE('',#13313,0.225);
#5265=CIRCLE('',#13314,0.225);
#5266=CIRCLE('',#13316,0.165);
#5267=CIRCLE('',#13318,0.165);
#5268=CIRCLE('',#13321,0.225);
#5269=CIRCLE('',#13323,0.225);
#5270=CIRCLE('',#13325,1.4);
#5271=CIRCLE('',#13327,0.605);
#5272=CIRCLE('',#13329,0.605);
#5273=CIRCLE('',#13331,2.);
#5274=CIRCLE('',#13339,1.4);
#5275=CIRCLE('',#13340,1.005);
#5276=CIRCLE('',#13342,1.005);
#5277=CIRCLE('',#13344,1.4);
#5278=CIRCLE('',#13346,1.6);
#5279=CIRCLE('',#13348,1.6);
#5280=CIRCLE('',#13352,0.225);
#5281=CIRCLE('',#13353,0.225);
#5282=CIRCLE('',#13355,0.225);
#5283=CIRCLE('',#13356,0.225);
#5284=CIRCLE('',#13364,1.01);
#5285=CIRCLE('',#13366,1.01);
#5286=CIRCLE('',#13377,1.4);
#5287=CIRCLE('',#13378,1.005);
#5288=CIRCLE('',#13380,1.005);
#5289=CIRCLE('',#13382,1.4);
#5290=CIRCLE('',#13384,1.6);
#5291=CIRCLE('',#13386,1.6);
#5292=CIRCLE('',#13390,0.225);
#5293=CIRCLE('',#13391,0.225);
#5294=CIRCLE('',#13393,0.225);
#5295=CIRCLE('',#13394,0.225);
#5296=CIRCLE('',#13402,1.01);
#5297=CIRCLE('',#13404,1.01);
#5298=CIRCLE('',#13413,0.5);
#5299=CIRCLE('',#13414,1.4);
#5300=CIRCLE('',#13418,0.605);
#5301=CIRCLE('',#13419,0.5);
#5302=CIRCLE('',#13421,0.165);
#5303=CIRCLE('',#13423,0.165);
#5304=CIRCLE('',#13427,0.605);
#5305=CIRCLE('',#13429,1.4);
#5306=CIRCLE('',#13433,0.165);
#5307=CIRCLE('',#13434,0.165);
#5308=CIRCLE('',#13436,0.165);
#5309=CIRCLE('',#13437,0.165);
#5310=CIRCLE('',#13439,0.165);
#5311=CIRCLE('',#13440,0.165);
#5312=CIRCLE('',#13442,0.165);
#5313=CIRCLE('',#13443,0.165);
#5314=CIRCLE('',#13445,0.225);
#5315=CIRCLE('',#13446,0.225);
#5316=CIRCLE('',#13448,0.225);
#5317=CIRCLE('',#13449,0.225);
#5318=CIRCLE('',#13451,1.6);
#5319=CIRCLE('',#13452,1.6);
#5320=CIRCLE('',#13465,0.225);
#5321=CIRCLE('',#13466,0.225);
#5322=CIRCLE('',#13468,0.225);
#5323=CIRCLE('',#13469,0.225);
#5324=CIRCLE('',#13471,0.225);
#5325=CIRCLE('',#13472,0.225);
#5326=CIRCLE('',#13474,0.225);
#5327=CIRCLE('',#13475,0.225);
#5328=CIRCLE('',#13477,1.59);
#5329=CIRCLE('',#13478,1.59);
#5330=CIRCLE('',#13480,1.41);
#5331=CIRCLE('',#13482,1.41);
#5332=CIRCLE('',#13484,2.4);
#5333=CIRCLE('',#13485,2.4);
#5334=CIRCLE('',#13490,0.225);
#5335=CIRCLE('',#13491,0.225);
#5336=CIRCLE('',#13493,0.225);
#5337=CIRCLE('',#13494,0.225);
#5338=CIRCLE('',#13496,0.225);
#5339=CIRCLE('',#13497,0.225);
#5340=CIRCLE('',#13499,0.225);
#5341=CIRCLE('',#13500,0.225);
#5342=CIRCLE('',#13502,1.59);
#5343=CIRCLE('',#13503,1.59);
#5344=CIRCLE('',#13505,1.41);
#5345=CIRCLE('',#13507,1.41);
#5346=CIRCLE('',#13509,2.4);
#5347=CIRCLE('',#13510,2.4);
#5348=CIRCLE('',#13515,0.165);
#5349=CIRCLE('',#13516,0.165);
#5350=CIRCLE('',#13518,0.165);
#5351=CIRCLE('',#13519,0.165);
#5352=CIRCLE('',#13521,0.165);
#5353=CIRCLE('',#13522,0.165);
#5354=CIRCLE('',#13524,0.165);
#5355=CIRCLE('',#13525,0.165);
#5356=CIRCLE('',#13527,0.225);
#5357=CIRCLE('',#13528,0.225);
#5358=CIRCLE('',#13530,0.225);
#5359=CIRCLE('',#13531,0.225);
#5360=CIRCLE('',#13533,1.6);
#5361=CIRCLE('',#13534,1.6);
#5362=CIRCLE('',#13547,0.225);
#5363=CIRCLE('',#13548,0.225);
#5364=CIRCLE('',#13550,0.225);
#5365=CIRCLE('',#13551,0.225);
#5366=CIRCLE('',#13553,0.225);
#5367=CIRCLE('',#13554,0.225);
#5368=CIRCLE('',#13556,0.225);
#5369=CIRCLE('',#13557,0.225);
#5370=CIRCLE('',#13559,1.59);
#5371=CIRCLE('',#13560,1.59);
#5372=CIRCLE('',#13562,1.41);
#5373=CIRCLE('',#13564,1.41);
#5374=CIRCLE('',#13566,2.4);
#5375=CIRCLE('',#13567,2.4);
#5376=CIRCLE('',#13572,0.225);
#5377=CIRCLE('',#13573,0.225);
#5378=CIRCLE('',#13575,0.225);
#5379=CIRCLE('',#13576,0.225);
#5380=CIRCLE('',#13578,0.225);
#5381=CIRCLE('',#13579,0.225);
#5382=CIRCLE('',#13581,0.225);
#5383=CIRCLE('',#13582,0.225);
#5384=CIRCLE('',#13584,1.59);
#5385=CIRCLE('',#13585,1.59);
#5386=CIRCLE('',#13587,1.41);
#5387=CIRCLE('',#13589,1.41);
#5388=CIRCLE('',#13591,2.4);
#5389=CIRCLE('',#13592,2.4);
#5390=CIRCLE('',#13597,0.6);
#5391=CIRCLE('',#13599,0.6);
#5392=CIRCLE('',#13600,0.5);
#5393=CIRCLE('',#13606,1.070235);
#5394=CIRCLE('',#13607,1.070235);
#5395=CIRCLE('',#13608,0.309556);
#5396=CIRCLE('',#13609,1.070235);
#5397=CIRCLE('',#13610,1.070235);
#5398=CIRCLE('',#13612,1.070235);
#5399=CIRCLE('',#13614,0.6);
#5400=CIRCLE('',#13615,0.6);
#5401=CIRCLE('',#13617,0.66);
#5402=CIRCLE('',#13620,1.070235);
#5403=CIRCLE('',#13622,0.66);
#5404=CIRCLE('',#13626,1.129765);
#5405=CIRCLE('',#13627,1.129765);
#5406=CIRCLE('',#13628,0.309556);
#5407=CIRCLE('',#13629,1.129765);
#5408=CIRCLE('',#13630,1.129765);
#5409=CIRCLE('',#13632,1.129765);
#5410=CIRCLE('',#13634,1.54);
#5411=CIRCLE('',#13635,1.129765);
#5412=CIRCLE('',#13637,1.6);
#5413=CIRCLE('',#13639,1.6);
#5414=CIRCLE('',#13641,1.54);
#5415=CIRCLE('',#13646,0.29765);
#5416=CIRCLE('',#13648,0.29765);
#5417=CIRCLE('',#13650,0.29765);
#5418=CIRCLE('',#13652,0.29765);
#5419=CIRCLE('',#13654,0.29765);
#5420=CIRCLE('',#13656,0.29765);
#5421=CIRCLE('',#13658,0.29765);
#5422=CIRCLE('',#13661,0.303778037777585);
#5423=CIRCLE('',#13662,0.303778037777585);
#5424=CIRCLE('',#13664,1.123812);
#5425=CIRCLE('',#13665,1.123812);
#5426=CIRCLE('',#13666,1.123812);
#5427=CIRCLE('',#13667,1.123812);
#5428=CIRCLE('',#13668,1.123812);
#5429=CIRCLE('',#13669,1.123812);
#5430=CIRCLE('',#13670,1.123812);
#5431=CIRCLE('',#13671,1.123812);
#5432=CIRCLE('',#13672,1.123812);
#5433=CIRCLE('',#13674,1.076188);
#5434=CIRCLE('',#13675,0.303778037777585);
#5435=CIRCLE('',#13677,0.303778037777585);
#5436=CIRCLE('',#13679,1.076188);
#5437=CIRCLE('',#13680,0.303778037777585);
#5438=CIRCLE('',#13682,0.303778037777585);
#5439=CIRCLE('',#13684,1.076188);
#5440=CIRCLE('',#13685,1.076188);
#5441=CIRCLE('',#13686,0.303778037777585);
#5442=CIRCLE('',#13688,0.303778037777585);
#5443=CIRCLE('',#13690,1.076188);
#5444=CIRCLE('',#13691,0.303778037777585);
#5445=CIRCLE('',#13693,0.303778037777585);
#5446=CIRCLE('',#13695,1.076188);
#5447=CIRCLE('',#13696,0.303778037777585);
#5448=CIRCLE('',#13698,0.303778037777585);
#5449=CIRCLE('',#13700,1.076188);
#5450=CIRCLE('',#13701,1.076188);
#5451=CIRCLE('',#13702,1.076188);
#5452=CIRCLE('',#13704,0.303778037777585);
#5453=CIRCLE('',#13706,0.303778037777585);
#5454=CIRCLE('',#13711,1.119765);
#5455=CIRCLE('',#13712,1.085235);
#5456=CIRCLE('',#13714,1.119765);
#5457=CIRCLE('',#13716,1.085235);
#5458=CIRCLE('',#13719,1.119765);
#5459=CIRCLE('',#13720,1.085235);
#5460=CIRCLE('',#13722,1.119765);
#5461=CIRCLE('',#13724,1.085235);
#5462=CIRCLE('',#13741,0.1954);
#5463=CIRCLE('',#13743,0.3);
#5464=CIRCLE('',#13745,0.35);
#5465=CIRCLE('',#13747,0.35);
#5466=CIRCLE('',#13749,0.32);
#5467=CIRCLE('',#13751,0.22);
#5468=CIRCLE('',#13753,0.1954);
#5469=CIRCLE('',#13758,0.425);
#5470=CIRCLE('',#13759,0.425);
#5471=CIRCLE('',#13764,1.);
#5472=CIRCLE('',#13765,1.);
#5473=CIRCLE('',#13767,1.);
#5474=CIRCLE('',#13768,1.);
#5475=CIRCLE('',#13933,1.);
#5476=CIRCLE('',#13934,1.);
#5477=CIRCLE('',#13939,0.164999999999999);
#5478=CIRCLE('',#13941,0.164999999999999);
#5479=CIRCLE('',#13944,0.3);
#5480=CIRCLE('',#13945,0.3);
#5481=CIRCLE('',#13947,0.5);
#5482=CIRCLE('',#13948,0.5);
#5483=CIRCLE('',#13951,1.4);
#5484=CIRCLE('',#13952,1.4);
#5485=CIRCLE('',#13957,0.3);
#5486=CIRCLE('',#13958,0.3);
#5487=CIRCLE('',#13963,0.199999999999999);
#5488=CIRCLE('',#13964,0.199999999999999);
#5489=CIRCLE('',#13974,1.005);
#5490=CIRCLE('',#13975,1.7);
#5491=CIRCLE('',#13977,1.7);
#5492=CIRCLE('',#13979,1.005);
#5493=CIRCLE('',#13990,0.17);
#5494=CIRCLE('',#13992,0.1954);
#5495=CIRCLE('',#13994,0.1954);
#5496=CIRCLE('',#13996,0.125);
#5497=CIRCLE('',#14007,0.165);
#5498=CIRCLE('',#14008,0.165);
#5499=CIRCLE('',#14011,0.165);
#5500=CIRCLE('',#14012,0.165);
#5501=CIRCLE('',#14016,0.6);
#5502=CIRCLE('',#14020,0.6);
#5503=CIRCLE('',#14023,0.6);
#5504=CIRCLE('',#14027,0.6);
#5505=CIRCLE('',#14029,0.6);
#5506=CIRCLE('',#14030,0.6);
#5507=CIRCLE('',#14035,0.605);
#5508=CIRCLE('',#14036,0.605);
#5509=CIRCLE('',#14038,0.8);
#5510=CIRCLE('',#14039,0.8);
#5511=CIRCLE('',#14044,0.605);
#5512=CIRCLE('',#14045,0.605);
#5513=CIRCLE('',#14047,0.8);
#5514=CIRCLE('',#14048,0.8);
#5515=CIRCLE('',#14053,0.605);
#5516=CIRCLE('',#14054,0.605);
#5517=CIRCLE('',#14056,0.8);
#5518=CIRCLE('',#14057,0.8);
#5519=CIRCLE('',#14062,0.605);
#5520=CIRCLE('',#14063,0.605);
#5521=CIRCLE('',#14065,0.8);
#5522=CIRCLE('',#14066,0.8);
#5523=CIRCLE('',#14085,0.25);
#5524=CIRCLE('',#14086,0.25);
#5525=CIRCLE('',#14091,1.3);
#5526=CIRCLE('',#14092,0.6);
#5527=CIRCLE('',#14094,0.6);
#5528=CIRCLE('',#14096,0.9);
#5529=CIRCLE('',#14097,0.9);
#5530=CIRCLE('',#14100,1.3);
#5531=CIRCLE('',#14103,1.3);
#5532=CIRCLE('',#14105,1.3);
#5533=CIRCLE('',#14109,0.33);
#5534=CIRCLE('',#14110,0.33);
#5535=CIRCLE('',#14112,0.4);
#5536=CIRCLE('',#14113,0.4);
#5537=CIRCLE('',#14118,0.225);
#5538=CIRCLE('',#14119,0.225);
#5539=CIRCLE('',#14121,1.);
#5540=CIRCLE('',#14122,1.);
#5541=CIRCLE('',#14127,0.225);
#5542=CIRCLE('',#14128,0.225);
#5543=CIRCLE('',#14130,1.);
#5544=CIRCLE('',#14131,1.);
#5545=CIRCLE('',#14139,1.75);
#5546=CIRCLE('',#14140,1.75);
#5547=CIRCLE('',#14141,1.75);
#5548=CIRCLE('',#14142,1.75);
#5549=CIRCLE('',#14143,1.75);
#5550=CIRCLE('',#14144,1.75);
#5551=CIRCLE('',#14145,1.75);
#5552=CIRCLE('',#14146,1.75);
#5553=CIRCLE('',#14147,1.75);
#5554=CIRCLE('',#14148,1.75);
#5555=CIRCLE('',#14149,1.75);
#5556=CIRCLE('',#14150,1.75);
#5557=CIRCLE('',#14151,1.75);
#5558=CIRCLE('',#14152,1.75);
#5559=CIRCLE('',#14153,1.75);
#5560=CIRCLE('',#14154,1.75);
#5561=CIRCLE('',#14155,1.75);
#5562=CIRCLE('',#14156,1.75);
#5563=CIRCLE('',#14157,1.75);
#5564=CIRCLE('',#14158,1.75);
#5565=CIRCLE('',#14159,0.6);
#5566=CIRCLE('',#14161,0.6);
#5567=CIRCLE('',#14163,1.4);
#5568=CIRCLE('',#14164,1.4);
#5569=CIRCLE('',#14168,1.75);
#5570=CIRCLE('',#14171,1.75);
#5571=CIRCLE('',#14174,1.75);
#5572=CIRCLE('',#14177,1.75);
#5573=CIRCLE('',#14180,1.75);
#5574=CIRCLE('',#14183,1.75);
#5575=CIRCLE('',#14186,1.75);
#5576=CIRCLE('',#14189,1.75);
#5577=CIRCLE('',#14192,1.75);
#5578=CIRCLE('',#14195,1.75);
#5579=CIRCLE('',#14198,1.75);
#5580=CIRCLE('',#14201,1.75);
#5581=CIRCLE('',#14204,1.75);
#5582=CIRCLE('',#14207,1.75);
#5583=CIRCLE('',#14210,1.75);
#5584=CIRCLE('',#14213,1.75);
#5585=CIRCLE('',#14216,1.75);
#5586=CIRCLE('',#14219,1.75);
#5587=CIRCLE('',#14222,1.75);
#5588=CIRCLE('',#14225,1.75);
#5589=CIRCLE('',#14229,0.32);
#5590=CIRCLE('',#14230,0.32);
#5591=CIRCLE('',#14232,0.6);
#5592=CIRCLE('',#14233,0.6);
#5593=CIRCLE('',#14238,0.45);
#5594=CIRCLE('',#14240,0.5);
#5595=CIRCLE('',#14242,0.5);
#5596=CIRCLE('',#14244,0.47);
#5597=CIRCLE('',#14246,0.32);
#5598=CIRCLE('',#14248,0.2942);
#5599=CIRCLE('',#14250,0.2942);
#5600=CIRCLE('',#14252,0.24);
#5601=CIRCLE('',#14264,0.3);
#5602=CIRCLE('',#14266,0.35);
#5603=CIRCLE('',#14268,0.35);
#5604=CIRCLE('',#14270,0.32);
#5605=CIRCLE('',#14272,0.22);
#5606=CIRCLE('',#14274,0.1954);
#5607=CIRCLE('',#14276,0.1954);
#5608=CIRCLE('',#14278,0.16);
#5609=CIRCLE('',#14355,0.405);
#5610=CIRCLE('',#14356,0.405);
#5611=CIRCLE('',#14358,0.9);
#5612=CIRCLE('',#14359,0.9);
#5613=VERTEX_POINT('',#17894);
#5614=VERTEX_POINT('',#17896);
#5615=VERTEX_POINT('',#17900);
#5616=VERTEX_POINT('',#17902);
#5617=VERTEX_POINT('',#17906);
#5618=VERTEX_POINT('',#17908);
#5619=VERTEX_POINT('',#17912);
#5620=VERTEX_POINT('',#17914);
#5621=VERTEX_POINT('',#17918);
#5622=VERTEX_POINT('',#17920);
#5623=VERTEX_POINT('',#17924);
#5624=VERTEX_POINT('',#17926);
#5625=VERTEX_POINT('',#17930);
#5626=VERTEX_POINT('',#17931);
#5627=VERTEX_POINT('',#17933);
#5628=VERTEX_POINT('',#17935);
#5629=VERTEX_POINT('',#17939);
#5630=VERTEX_POINT('',#17941);
#5631=VERTEX_POINT('',#17945);
#5632=VERTEX_POINT('',#17947);
#5633=VERTEX_POINT('',#17957);
#5634=VERTEX_POINT('',#17958);
#5635=VERTEX_POINT('',#17960);
#5636=VERTEX_POINT('',#17962);
#5637=VERTEX_POINT('',#17966);
#5638=VERTEX_POINT('',#17968);
#5639=VERTEX_POINT('',#17972);
#5640=VERTEX_POINT('',#17974);
#5641=VERTEX_POINT('',#17984);
#5642=VERTEX_POINT('',#17985);
#5643=VERTEX_POINT('',#17987);
#5644=VERTEX_POINT('',#17989);
#5645=VERTEX_POINT('',#17993);
#5646=VERTEX_POINT('',#17995);
#5647=VERTEX_POINT('',#17999);
#5648=VERTEX_POINT('',#18001);
#5649=VERTEX_POINT('',#18011);
#5650=VERTEX_POINT('',#18013);
#5651=VERTEX_POINT('',#18018);
#5652=VERTEX_POINT('',#18020);
#5653=VERTEX_POINT('',#18025);
#5654=VERTEX_POINT('',#18026);
#5655=VERTEX_POINT('',#18028);
#5656=VERTEX_POINT('',#18030);
#5657=VERTEX_POINT('',#18034);
#5658=VERTEX_POINT('',#18035);
#5659=VERTEX_POINT('',#18037);
#5660=VERTEX_POINT('',#18039);
#5661=VERTEX_POINT('',#18043);
#5662=VERTEX_POINT('',#18045);
#5663=VERTEX_POINT('',#18047);
#5664=VERTEX_POINT('',#18049);
#5665=VERTEX_POINT('',#18056);
#5666=VERTEX_POINT('',#18060);
#5667=VERTEX_POINT('',#18064);
#5668=VERTEX_POINT('',#18066);
#5669=VERTEX_POINT('',#18074);
#5670=VERTEX_POINT('',#18076);
#5671=VERTEX_POINT('',#18081);
#5672=VERTEX_POINT('',#18083);
#5673=VERTEX_POINT('',#18088);
#5674=VERTEX_POINT('',#18089);
#5675=VERTEX_POINT('',#18091);
#5676=VERTEX_POINT('',#18093);
#5677=VERTEX_POINT('',#18097);
#5678=VERTEX_POINT('',#18098);
#5679=VERTEX_POINT('',#18100);
#5680=VERTEX_POINT('',#18102);
#5681=VERTEX_POINT('',#18106);
#5682=VERTEX_POINT('',#18108);
#5683=VERTEX_POINT('',#18110);
#5684=VERTEX_POINT('',#18112);
#5685=VERTEX_POINT('',#18114);
#5686=VERTEX_POINT('',#18116);
#5687=VERTEX_POINT('',#18118);
#5688=VERTEX_POINT('',#18120);
#5689=VERTEX_POINT('',#18122);
#5690=VERTEX_POINT('',#18124);
#5691=VERTEX_POINT('',#18126);
#5692=VERTEX_POINT('',#18133);
#5693=VERTEX_POINT('',#18137);
#5694=VERTEX_POINT('',#18141);
#5695=VERTEX_POINT('',#18143);
#5696=VERTEX_POINT('',#18151);
#5697=VERTEX_POINT('',#18153);
#5698=VERTEX_POINT('',#18157);
#5699=VERTEX_POINT('',#18158);
#5700=VERTEX_POINT('',#18162);
#5701=VERTEX_POINT('',#18177);
#5702=VERTEX_POINT('',#18179);
#5703=VERTEX_POINT('',#18188);
#5704=VERTEX_POINT('',#18190);
#5705=VERTEX_POINT('',#18241);
#5706=VERTEX_POINT('',#18243);
#5707=VERTEX_POINT('',#18247);
#5708=VERTEX_POINT('',#18252);
#5709=VERTEX_POINT('',#18256);
#5710=VERTEX_POINT('',#18265);
#5711=VERTEX_POINT('',#18266);
#5712=VERTEX_POINT('',#18268);
#5713=VERTEX_POINT('',#18270);
#5714=VERTEX_POINT('',#18276);
#5715=VERTEX_POINT('',#18277);
#5716=VERTEX_POINT('',#18279);
#5717=VERTEX_POINT('',#18281);
#5718=VERTEX_POINT('',#18287);
#5719=VERTEX_POINT('',#18289);
#5720=VERTEX_POINT('',#18293);
#5721=VERTEX_POINT('',#18295);
#5722=VERTEX_POINT('',#18298);
#5723=VERTEX_POINT('',#18299);
#5724=VERTEX_POINT('',#18303);
#5725=VERTEX_POINT('',#18318);
#5726=VERTEX_POINT('',#18320);
#5727=VERTEX_POINT('',#18329);
#5728=VERTEX_POINT('',#18331);
#5729=VERTEX_POINT('',#18379);
#5730=VERTEX_POINT('',#18383);
#5731=VERTEX_POINT('',#18387);
#5732=VERTEX_POINT('',#18391);
#5733=VERTEX_POINT('',#18394);
#5734=VERTEX_POINT('',#18398);
#5735=VERTEX_POINT('',#18404);
#5736=VERTEX_POINT('',#18405);
#5737=VERTEX_POINT('',#18407);
#5738=VERTEX_POINT('',#18409);
#5739=VERTEX_POINT('',#18413);
#5740=VERTEX_POINT('',#18414);
#5741=VERTEX_POINT('',#18416);
#5742=VERTEX_POINT('',#18418);
#5743=VERTEX_POINT('',#18422);
#5744=VERTEX_POINT('',#18424);
#5745=VERTEX_POINT('',#18426);
#5746=VERTEX_POINT('',#18428);
#5747=VERTEX_POINT('',#18432);
#5748=VERTEX_POINT('',#18434);
#5749=VERTEX_POINT('',#18436);
#5750=VERTEX_POINT('',#18438);
#5751=VERTEX_POINT('',#18455);
#5752=VERTEX_POINT('',#18457);
#5753=VERTEX_POINT('',#18461);
#5754=VERTEX_POINT('',#18463);
#5755=VERTEX_POINT('',#18467);
#5756=VERTEX_POINT('',#18468);
#5757=VERTEX_POINT('',#18470);
#5758=VERTEX_POINT('',#18472);
#5759=VERTEX_POINT('',#18476);
#5760=VERTEX_POINT('',#18477);
#5761=VERTEX_POINT('',#18479);
#5762=VERTEX_POINT('',#18481);
#5763=VERTEX_POINT('',#18485);
#5764=VERTEX_POINT('',#18487);
#5765=VERTEX_POINT('',#18491);
#5766=VERTEX_POINT('',#18493);
#5767=VERTEX_POINT('',#18497);
#5768=VERTEX_POINT('',#18499);
#5769=VERTEX_POINT('',#18503);
#5770=VERTEX_POINT('',#18505);
#5771=VERTEX_POINT('',#18510);
#5772=VERTEX_POINT('',#18512);
#5773=VERTEX_POINT('',#18518);
#5774=VERTEX_POINT('',#18522);
#5775=VERTEX_POINT('',#18530);
#5776=VERTEX_POINT('',#18531);
#5777=VERTEX_POINT('',#18533);
#5778=VERTEX_POINT('',#18535);
#5779=VERTEX_POINT('',#18539);
#5780=VERTEX_POINT('',#18540);
#5781=VERTEX_POINT('',#18542);
#5782=VERTEX_POINT('',#18544);
#5783=VERTEX_POINT('',#18548);
#5784=VERTEX_POINT('',#18550);
#5785=VERTEX_POINT('',#18552);
#5786=VERTEX_POINT('',#18554);
#5787=VERTEX_POINT('',#18558);
#5788=VERTEX_POINT('',#18560);
#5789=VERTEX_POINT('',#18562);
#5790=VERTEX_POINT('',#18564);
#5791=VERTEX_POINT('',#18581);
#5792=VERTEX_POINT('',#18583);
#5793=VERTEX_POINT('',#18587);
#5794=VERTEX_POINT('',#18589);
#5795=VERTEX_POINT('',#18593);
#5796=VERTEX_POINT('',#18594);
#5797=VERTEX_POINT('',#18596);
#5798=VERTEX_POINT('',#18598);
#5799=VERTEX_POINT('',#18602);
#5800=VERTEX_POINT('',#18603);
#5801=VERTEX_POINT('',#18605);
#5802=VERTEX_POINT('',#18607);
#5803=VERTEX_POINT('',#18611);
#5804=VERTEX_POINT('',#18613);
#5805=VERTEX_POINT('',#18617);
#5806=VERTEX_POINT('',#18619);
#5807=VERTEX_POINT('',#18623);
#5808=VERTEX_POINT('',#18625);
#5809=VERTEX_POINT('',#18629);
#5810=VERTEX_POINT('',#18631);
#5811=VERTEX_POINT('',#18636);
#5812=VERTEX_POINT('',#18638);
#5813=VERTEX_POINT('',#18644);
#5814=VERTEX_POINT('',#18648);
#5815=VERTEX_POINT('',#18656);
#5816=VERTEX_POINT('',#18657);
#5817=VERTEX_POINT('',#18659);
#5818=VERTEX_POINT('',#18661);
#5819=VERTEX_POINT('',#18665);
#5820=VERTEX_POINT('',#18667);
#5821=VERTEX_POINT('',#18671);
#5822=VERTEX_POINT('',#18674);
#5823=VERTEX_POINT('',#18676);
#5824=VERTEX_POINT('',#18679);
#5825=VERTEX_POINT('',#18685);
#5826=VERTEX_POINT('',#18687);
#5827=VERTEX_POINT('',#18690);
#5828=VERTEX_POINT('',#18691);
#5829=VERTEX_POINT('',#18695);
#5830=VERTEX_POINT('',#18710);
#5831=VERTEX_POINT('',#18712);
#5832=VERTEX_POINT('',#18721);
#5833=VERTEX_POINT('',#18723);
#5834=VERTEX_POINT('',#18773);
#5835=VERTEX_POINT('',#18777);
#5836=VERTEX_POINT('',#18783);
#5837=VERTEX_POINT('',#18785);
#5838=VERTEX_POINT('',#18789);
#5839=VERTEX_POINT('',#18791);
#5840=VERTEX_POINT('',#18795);
#5841=VERTEX_POINT('',#18797);
#5842=VERTEX_POINT('',#18801);
#5843=VERTEX_POINT('',#18803);
#5844=VERTEX_POINT('',#18807);
#5845=VERTEX_POINT('',#18809);
#5846=VERTEX_POINT('',#18813);
#5847=VERTEX_POINT('',#18815);
#5848=VERTEX_POINT('',#18819);
#5849=VERTEX_POINT('',#18821);
#5850=VERTEX_POINT('',#18825);
#5851=VERTEX_POINT('',#18826);
#5852=VERTEX_POINT('',#18828);
#5853=VERTEX_POINT('',#18830);
#5854=VERTEX_POINT('',#18834);
#5855=VERTEX_POINT('',#18835);
#5856=VERTEX_POINT('',#18837);
#5857=VERTEX_POINT('',#18839);
#5858=VERTEX_POINT('',#18843);
#5859=VERTEX_POINT('',#18845);
#5860=VERTEX_POINT('',#18849);
#5861=VERTEX_POINT('',#18851);
#5862=VERTEX_POINT('',#18855);
#5863=VERTEX_POINT('',#18857);
#5864=VERTEX_POINT('',#18862);
#5865=VERTEX_POINT('',#18866);
#5866=VERTEX_POINT('',#18876);
#5867=VERTEX_POINT('',#18878);
#5868=VERTEX_POINT('',#18882);
#5869=VERTEX_POINT('',#18884);
#5870=VERTEX_POINT('',#18888);
#5871=VERTEX_POINT('',#18890);
#5872=VERTEX_POINT('',#18894);
#5873=VERTEX_POINT('',#18896);
#5874=VERTEX_POINT('',#18900);
#5875=VERTEX_POINT('',#18902);
#5876=VERTEX_POINT('',#18906);
#5877=VERTEX_POINT('',#18909);
#5878=VERTEX_POINT('',#18913);
#5879=VERTEX_POINT('',#18915);
#5880=VERTEX_POINT('',#18922);
#5881=VERTEX_POINT('',#18924);
#5882=VERTEX_POINT('',#18928);
#5883=VERTEX_POINT('',#18930);
#5884=VERTEX_POINT('',#18934);
#5885=VERTEX_POINT('',#18936);
#5886=VERTEX_POINT('',#18940);
#5887=VERTEX_POINT('',#18942);
#5888=VERTEX_POINT('',#18946);
#5889=VERTEX_POINT('',#18948);
#5890=VERTEX_POINT('',#18952);
#5891=VERTEX_POINT('',#18955);
#5892=VERTEX_POINT('',#18959);
#5893=VERTEX_POINT('',#18961);
#5894=VERTEX_POINT('',#18968);
#5895=VERTEX_POINT('',#18970);
#5896=VERTEX_POINT('',#18974);
#5897=VERTEX_POINT('',#18976);
#5898=VERTEX_POINT('',#18980);
#5899=VERTEX_POINT('',#18982);
#5900=VERTEX_POINT('',#18986);
#5901=VERTEX_POINT('',#18988);
#5902=VERTEX_POINT('',#18992);
#5903=VERTEX_POINT('',#18994);
#5904=VERTEX_POINT('',#18998);
#5905=VERTEX_POINT('',#19000);
#5906=VERTEX_POINT('',#19004);
#5907=VERTEX_POINT('',#19006);
#5908=VERTEX_POINT('',#19010);
#5909=VERTEX_POINT('',#19011);
#5910=VERTEX_POINT('',#19013);
#5911=VERTEX_POINT('',#19015);
#5912=VERTEX_POINT('',#19019);
#5913=VERTEX_POINT('',#19020);
#5914=VERTEX_POINT('',#19022);
#5915=VERTEX_POINT('',#19024);
#5916=VERTEX_POINT('',#19028);
#5917=VERTEX_POINT('',#19030);
#5918=VERTEX_POINT('',#19034);
#5919=VERTEX_POINT('',#19036);
#5920=VERTEX_POINT('',#19040);
#5921=VERTEX_POINT('',#19042);
#5922=VERTEX_POINT('',#19047);
#5923=VERTEX_POINT('',#19051);
#5924=VERTEX_POINT('',#19061);
#5925=VERTEX_POINT('',#19063);
#5926=VERTEX_POINT('',#19067);
#5927=VERTEX_POINT('',#19069);
#5928=VERTEX_POINT('',#19073);
#5929=VERTEX_POINT('',#19075);
#5930=VERTEX_POINT('',#19079);
#5931=VERTEX_POINT('',#19081);
#5932=VERTEX_POINT('',#19085);
#5933=VERTEX_POINT('',#19087);
#5934=VERTEX_POINT('',#19091);
#5935=VERTEX_POINT('',#19094);
#5936=VERTEX_POINT('',#19098);
#5937=VERTEX_POINT('',#19100);
#5938=VERTEX_POINT('',#19107);
#5939=VERTEX_POINT('',#19109);
#5940=VERTEX_POINT('',#19113);
#5941=VERTEX_POINT('',#19115);
#5942=VERTEX_POINT('',#19119);
#5943=VERTEX_POINT('',#19121);
#5944=VERTEX_POINT('',#19125);
#5945=VERTEX_POINT('',#19127);
#5946=VERTEX_POINT('',#19131);
#5947=VERTEX_POINT('',#19133);
#5948=VERTEX_POINT('',#19137);
#5949=VERTEX_POINT('',#19140);
#5950=VERTEX_POINT('',#19144);
#5951=VERTEX_POINT('',#19146);
#5952=VERTEX_POINT('',#19153);
#5953=VERTEX_POINT('',#19156);
#5954=VERTEX_POINT('',#19158);
#5955=VERTEX_POINT('',#19167);
#5956=VERTEX_POINT('',#19168);
#5957=VERTEX_POINT('',#19171);
#5958=VERTEX_POINT('',#19173);
#5959=VERTEX_POINT('',#19177);
#5960=VERTEX_POINT('',#19181);
#5961=VERTEX_POINT('',#19183);
#5962=VERTEX_POINT('',#19187);
#5963=VERTEX_POINT('',#19192);
#5964=VERTEX_POINT('',#19196);
#5965=VERTEX_POINT('',#19202);
#5966=VERTEX_POINT('',#19203);
#5967=VERTEX_POINT('',#19206);
#5968=VERTEX_POINT('',#19208);
#5969=VERTEX_POINT('',#19212);
#5970=VERTEX_POINT('',#19216);
#5971=VERTEX_POINT('',#19218);
#5972=VERTEX_POINT('',#19221);
#5973=VERTEX_POINT('',#19225);
#5974=VERTEX_POINT('',#19229);
#5975=VERTEX_POINT('',#19237);
#5976=VERTEX_POINT('',#19238);
#5977=VERTEX_POINT('',#19241);
#5978=VERTEX_POINT('',#19242);
#5979=VERTEX_POINT('',#19245);
#5980=VERTEX_POINT('',#19246);
#5981=VERTEX_POINT('',#19249);
#5982=VERTEX_POINT('',#19250);
#5983=VERTEX_POINT('',#19253);
#5984=VERTEX_POINT('',#19254);
#5985=VERTEX_POINT('',#19257);
#5986=VERTEX_POINT('',#19258);
#5987=VERTEX_POINT('',#19261);
#5988=VERTEX_POINT('',#19262);
#5989=VERTEX_POINT('',#19266);
#5990=VERTEX_POINT('',#19267);
#5991=VERTEX_POINT('',#19290);
#5992=VERTEX_POINT('',#19292);
#5993=VERTEX_POINT('',#19317);
#5994=VERTEX_POINT('',#19319);
#5995=VERTEX_POINT('',#19342);
#5996=VERTEX_POINT('',#19344);
#5997=VERTEX_POINT('',#19367);
#5998=VERTEX_POINT('',#19369);
#5999=VERTEX_POINT('',#19372);
#6000=VERTEX_POINT('',#19374);
#6001=VERTEX_POINT('',#19397);
#6002=VERTEX_POINT('',#19399);
#6003=VERTEX_POINT('',#19422);
#6004=VERTEX_POINT('',#19424);
#6005=VERTEX_POINT('',#19447);
#6006=VERTEX_POINT('',#19449);
#6007=VERTEX_POINT('',#19474);
#6008=VERTEX_POINT('',#19478);
#6009=VERTEX_POINT('',#19503);
#6010=VERTEX_POINT('',#19507);
#6011=VERTEX_POINT('',#19532);
#6012=VERTEX_POINT('',#19534);
#6013=VERTEX_POINT('',#19538);
#6014=VERTEX_POINT('',#19563);
#6015=VERTEX_POINT('',#19567);
#6016=VERTEX_POINT('',#19592);
#6017=VERTEX_POINT('',#19596);
#6018=VERTEX_POINT('',#19621);
#6019=VERTEX_POINT('',#19624);
#6020=VERTEX_POINT('',#19626);
#6021=VERTEX_POINT('',#19658);
#6022=VERTEX_POINT('',#19660);
#6023=VERTEX_POINT('',#19663);
#6024=VERTEX_POINT('',#19667);
#6025=VERTEX_POINT('',#19672);
#6026=VERTEX_POINT('',#19674);
#6027=VERTEX_POINT('',#19677);
#6028=VERTEX_POINT('',#19681);
#6029=VERTEX_POINT('',#19692);
#6030=VERTEX_POINT('',#19693);
#6031=VERTEX_POINT('',#19695);
#6032=VERTEX_POINT('',#19697);
#6033=VERTEX_POINT('',#19701);
#6034=VERTEX_POINT('',#19703);
#6035=VERTEX_POINT('',#19707);
#6036=VERTEX_POINT('',#19709);
#6037=VERTEX_POINT('',#19713);
#6038=VERTEX_POINT('',#19715);
#6039=VERTEX_POINT('',#19719);
#6040=VERTEX_POINT('',#19721);
#6041=VERTEX_POINT('',#19730);
#6042=VERTEX_POINT('',#19733);
#6043=VERTEX_POINT('',#19736);
#6044=VERTEX_POINT('',#19740);
#6045=VERTEX_POINT('',#19744);
#6046=VERTEX_POINT('',#19748);
#6047=VERTEX_POINT('',#19751);
#6048=VERTEX_POINT('',#19759);
#6049=VERTEX_POINT('',#19761);
#6050=VERTEX_POINT('',#19766);
#6051=VERTEX_POINT('',#19767);
#6052=VERTEX_POINT('',#19769);
#6053=VERTEX_POINT('',#19771);
#6054=VERTEX_POINT('',#19775);
#6055=VERTEX_POINT('',#19776);
#6056=VERTEX_POINT('',#19778);
#6057=VERTEX_POINT('',#19780);
#6058=VERTEX_POINT('',#19784);
#6059=VERTEX_POINT('',#19786);
#6060=VERTEX_POINT('',#19788);
#6061=VERTEX_POINT('',#19793);
#6062=VERTEX_POINT('',#19795);
#6063=VERTEX_POINT('',#19797);
#6064=VERTEX_POINT('',#19802);
#6065=VERTEX_POINT('',#19804);
#6066=VERTEX_POINT('',#19808);
#6067=VERTEX_POINT('',#19810);
#6068=VERTEX_POINT('',#19814);
#6069=VERTEX_POINT('',#19816);
#6070=VERTEX_POINT('',#19820);
#6071=VERTEX_POINT('',#19822);
#6072=VERTEX_POINT('',#19826);
#6073=VERTEX_POINT('',#19828);
#6074=VERTEX_POINT('',#19832);
#6075=VERTEX_POINT('',#19834);
#6076=VERTEX_POINT('',#19838);
#6077=VERTEX_POINT('',#19840);
#6078=VERTEX_POINT('',#19844);
#6079=VERTEX_POINT('',#19846);
#6080=VERTEX_POINT('',#19850);
#6081=VERTEX_POINT('',#19852);
#6082=VERTEX_POINT('',#19856);
#6083=VERTEX_POINT('',#19858);
#6084=VERTEX_POINT('',#19862);
#6085=VERTEX_POINT('',#19864);
#6086=VERTEX_POINT('',#19868);
#6087=VERTEX_POINT('',#19870);
#6088=VERTEX_POINT('',#19874);
#6089=VERTEX_POINT('',#19876);
#6090=VERTEX_POINT('',#19880);
#6091=VERTEX_POINT('',#19882);
#6092=VERTEX_POINT('',#19886);
#6093=VERTEX_POINT('',#19888);
#6094=VERTEX_POINT('',#19892);
#6095=VERTEX_POINT('',#19894);
#6096=VERTEX_POINT('',#19898);
#6097=VERTEX_POINT('',#19900);
#6098=VERTEX_POINT('',#19904);
#6099=VERTEX_POINT('',#19906);
#6100=VERTEX_POINT('',#19910);
#6101=VERTEX_POINT('',#19912);
#6102=VERTEX_POINT('',#19916);
#6103=VERTEX_POINT('',#19918);
#6104=VERTEX_POINT('',#19922);
#6105=VERTEX_POINT('',#19924);
#6106=VERTEX_POINT('',#19928);
#6107=VERTEX_POINT('',#19930);
#6108=VERTEX_POINT('',#19934);
#6109=VERTEX_POINT('',#19936);
#6110=VERTEX_POINT('',#19940);
#6111=VERTEX_POINT('',#19942);
#6112=VERTEX_POINT('',#19946);
#6113=VERTEX_POINT('',#19948);
#6114=VERTEX_POINT('',#19952);
#6115=VERTEX_POINT('',#19954);
#6116=VERTEX_POINT('',#19958);
#6117=VERTEX_POINT('',#19960);
#6118=VERTEX_POINT('',#19964);
#6119=VERTEX_POINT('',#19966);
#6120=VERTEX_POINT('',#19970);
#6121=VERTEX_POINT('',#19972);
#6122=VERTEX_POINT('',#19976);
#6123=VERTEX_POINT('',#19978);
#6124=VERTEX_POINT('',#19982);
#6125=VERTEX_POINT('',#19984);
#6126=VERTEX_POINT('',#19988);
#6127=VERTEX_POINT('',#19990);
#6128=VERTEX_POINT('',#19994);
#6129=VERTEX_POINT('',#19996);
#6130=VERTEX_POINT('',#20000);
#6131=VERTEX_POINT('',#20002);
#6132=VERTEX_POINT('',#20006);
#6133=VERTEX_POINT('',#20008);
#6134=VERTEX_POINT('',#20012);
#6135=VERTEX_POINT('',#20014);
#6136=VERTEX_POINT('',#20018);
#6137=VERTEX_POINT('',#20020);
#6138=VERTEX_POINT('',#20024);
#6139=VERTEX_POINT('',#20026);
#6140=VERTEX_POINT('',#20030);
#6141=VERTEX_POINT('',#20032);
#6142=VERTEX_POINT('',#20036);
#6143=VERTEX_POINT('',#20038);
#6144=VERTEX_POINT('',#20042);
#6145=VERTEX_POINT('',#20044);
#6146=VERTEX_POINT('',#20048);
#6147=VERTEX_POINT('',#20050);
#6148=VERTEX_POINT('',#20054);
#6149=VERTEX_POINT('',#20056);
#6150=VERTEX_POINT('',#20060);
#6151=VERTEX_POINT('',#20062);
#6152=VERTEX_POINT('',#20066);
#6153=VERTEX_POINT('',#20068);
#6154=VERTEX_POINT('',#20072);
#6155=VERTEX_POINT('',#20074);
#6156=VERTEX_POINT('',#20078);
#6157=VERTEX_POINT('',#20080);
#6158=VERTEX_POINT('',#20084);
#6159=VERTEX_POINT('',#20086);
#6160=VERTEX_POINT('',#20090);
#6161=VERTEX_POINT('',#20092);
#6162=VERTEX_POINT('',#20096);
#6163=VERTEX_POINT('',#20098);
#6164=VERTEX_POINT('',#20102);
#6165=VERTEX_POINT('',#20104);
#6166=VERTEX_POINT('',#20108);
#6167=VERTEX_POINT('',#20110);
#6168=VERTEX_POINT('',#20114);
#6169=VERTEX_POINT('',#20116);
#6170=VERTEX_POINT('',#20120);
#6171=VERTEX_POINT('',#20122);
#6172=VERTEX_POINT('',#20126);
#6173=VERTEX_POINT('',#20128);
#6174=VERTEX_POINT('',#20132);
#6175=VERTEX_POINT('',#20134);
#6176=VERTEX_POINT('',#20138);
#6177=VERTEX_POINT('',#20140);
#6178=VERTEX_POINT('',#20144);
#6179=VERTEX_POINT('',#20146);
#6180=VERTEX_POINT('',#20150);
#6181=VERTEX_POINT('',#20152);
#6182=VERTEX_POINT('',#20156);
#6183=VERTEX_POINT('',#20158);
#6184=VERTEX_POINT('',#20162);
#6185=VERTEX_POINT('',#20164);
#6186=VERTEX_POINT('',#20168);
#6187=VERTEX_POINT('',#20170);
#6188=VERTEX_POINT('',#20174);
#6189=VERTEX_POINT('',#20176);
#6190=VERTEX_POINT('',#20180);
#6191=VERTEX_POINT('',#20182);
#6192=VERTEX_POINT('',#20186);
#6193=VERTEX_POINT('',#20188);
#6194=VERTEX_POINT('',#20192);
#6195=VERTEX_POINT('',#20194);
#6196=VERTEX_POINT('',#20198);
#6197=VERTEX_POINT('',#20200);
#6198=VERTEX_POINT('',#20204);
#6199=VERTEX_POINT('',#20206);
#6200=VERTEX_POINT('',#20210);
#6201=VERTEX_POINT('',#20212);
#6202=VERTEX_POINT('',#20216);
#6203=VERTEX_POINT('',#20218);
#6204=VERTEX_POINT('',#20222);
#6205=VERTEX_POINT('',#20224);
#6206=VERTEX_POINT('',#20228);
#6207=VERTEX_POINT('',#20230);
#6208=VERTEX_POINT('',#20234);
#6209=VERTEX_POINT('',#20236);
#6210=VERTEX_POINT('',#20240);
#6211=VERTEX_POINT('',#20242);
#6212=VERTEX_POINT('',#20246);
#6213=VERTEX_POINT('',#20248);
#6214=VERTEX_POINT('',#20252);
#6215=VERTEX_POINT('',#20254);
#6216=VERTEX_POINT('',#20258);
#6217=VERTEX_POINT('',#20260);
#6218=VERTEX_POINT('',#20264);
#6219=VERTEX_POINT('',#20266);
#6220=VERTEX_POINT('',#20270);
#6221=VERTEX_POINT('',#20272);
#6222=VERTEX_POINT('',#20276);
#6223=VERTEX_POINT('',#20278);
#6224=VERTEX_POINT('',#20282);
#6225=VERTEX_POINT('',#20284);
#6226=VERTEX_POINT('',#20288);
#6227=VERTEX_POINT('',#20290);
#6228=VERTEX_POINT('',#20294);
#6229=VERTEX_POINT('',#20296);
#6230=VERTEX_POINT('',#20300);
#6231=VERTEX_POINT('',#20302);
#6232=VERTEX_POINT('',#20306);
#6233=VERTEX_POINT('',#20308);
#6234=VERTEX_POINT('',#20312);
#6235=VERTEX_POINT('',#20314);
#6236=VERTEX_POINT('',#20318);
#6237=VERTEX_POINT('',#20320);
#6238=VERTEX_POINT('',#20324);
#6239=VERTEX_POINT('',#20326);
#6240=VERTEX_POINT('',#20330);
#6241=VERTEX_POINT('',#20332);
#6242=VERTEX_POINT('',#20336);
#6243=VERTEX_POINT('',#20338);
#6244=VERTEX_POINT('',#20342);
#6245=VERTEX_POINT('',#20344);
#6246=VERTEX_POINT('',#20348);
#6247=VERTEX_POINT('',#20350);
#6248=VERTEX_POINT('',#20354);
#6249=VERTEX_POINT('',#20356);
#6250=VERTEX_POINT('',#20360);
#6251=VERTEX_POINT('',#20362);
#6252=VERTEX_POINT('',#20366);
#6253=VERTEX_POINT('',#20368);
#6254=VERTEX_POINT('',#20372);
#6255=VERTEX_POINT('',#20374);
#6256=VERTEX_POINT('',#20378);
#6257=VERTEX_POINT('',#20380);
#6258=VERTEX_POINT('',#20384);
#6259=VERTEX_POINT('',#20386);
#6260=VERTEX_POINT('',#20390);
#6261=VERTEX_POINT('',#20392);
#6262=VERTEX_POINT('',#20396);
#6263=VERTEX_POINT('',#20398);
#6264=VERTEX_POINT('',#20402);
#6265=VERTEX_POINT('',#20404);
#6266=VERTEX_POINT('',#20408);
#6267=VERTEX_POINT('',#20410);
#6268=VERTEX_POINT('',#20414);
#6269=VERTEX_POINT('',#20416);
#6270=VERTEX_POINT('',#20420);
#6271=VERTEX_POINT('',#20422);
#6272=VERTEX_POINT('',#20426);
#6273=VERTEX_POINT('',#20428);
#6274=VERTEX_POINT('',#20432);
#6275=VERTEX_POINT('',#20434);
#6276=VERTEX_POINT('',#20438);
#6277=VERTEX_POINT('',#20440);
#6278=VERTEX_POINT('',#20444);
#6279=VERTEX_POINT('',#20446);
#6280=VERTEX_POINT('',#20450);
#6281=VERTEX_POINT('',#20452);
#6282=VERTEX_POINT('',#20456);
#6283=VERTEX_POINT('',#20458);
#6284=VERTEX_POINT('',#20462);
#6285=VERTEX_POINT('',#20464);
#6286=VERTEX_POINT('',#20468);
#6287=VERTEX_POINT('',#20470);
#6288=VERTEX_POINT('',#20474);
#6289=VERTEX_POINT('',#20476);
#6290=VERTEX_POINT('',#20480);
#6291=VERTEX_POINT('',#20482);
#6292=VERTEX_POINT('',#20486);
#6293=VERTEX_POINT('',#20488);
#6294=VERTEX_POINT('',#20492);
#6295=VERTEX_POINT('',#20494);
#6296=VERTEX_POINT('',#20498);
#6297=VERTEX_POINT('',#20500);
#6298=VERTEX_POINT('',#20504);
#6299=VERTEX_POINT('',#20506);
#6300=VERTEX_POINT('',#20510);
#6301=VERTEX_POINT('',#20512);
#6302=VERTEX_POINT('',#20516);
#6303=VERTEX_POINT('',#20518);
#6304=VERTEX_POINT('',#20522);
#6305=VERTEX_POINT('',#20524);
#6306=VERTEX_POINT('',#20528);
#6307=VERTEX_POINT('',#20530);
#6308=VERTEX_POINT('',#20534);
#6309=VERTEX_POINT('',#20536);
#6310=VERTEX_POINT('',#20540);
#6311=VERTEX_POINT('',#20542);
#6312=VERTEX_POINT('',#20546);
#6313=VERTEX_POINT('',#20548);
#6314=VERTEX_POINT('',#20552);
#6315=VERTEX_POINT('',#20554);
#6316=VERTEX_POINT('',#20558);
#6317=VERTEX_POINT('',#20560);
#6318=VERTEX_POINT('',#20564);
#6319=VERTEX_POINT('',#20566);
#6320=VERTEX_POINT('',#20570);
#6321=VERTEX_POINT('',#20572);
#6322=VERTEX_POINT('',#20576);
#6323=VERTEX_POINT('',#20578);
#6324=VERTEX_POINT('',#20582);
#6325=VERTEX_POINT('',#20584);
#6326=VERTEX_POINT('',#20588);
#6327=VERTEX_POINT('',#20590);
#6328=VERTEX_POINT('',#20594);
#6329=VERTEX_POINT('',#20596);
#6330=VERTEX_POINT('',#20600);
#6331=VERTEX_POINT('',#20602);
#6332=VERTEX_POINT('',#20606);
#6333=VERTEX_POINT('',#20608);
#6334=VERTEX_POINT('',#20612);
#6335=VERTEX_POINT('',#20614);
#6336=VERTEX_POINT('',#20618);
#6337=VERTEX_POINT('',#20620);
#6338=VERTEX_POINT('',#20624);
#6339=VERTEX_POINT('',#20626);
#6340=VERTEX_POINT('',#20630);
#6341=VERTEX_POINT('',#20632);
#6342=VERTEX_POINT('',#20636);
#6343=VERTEX_POINT('',#20638);
#6344=VERTEX_POINT('',#20642);
#6345=VERTEX_POINT('',#20644);
#6346=VERTEX_POINT('',#20648);
#6347=VERTEX_POINT('',#20650);
#6348=VERTEX_POINT('',#20654);
#6349=VERTEX_POINT('',#20656);
#6350=VERTEX_POINT('',#20660);
#6351=VERTEX_POINT('',#20662);
#6352=VERTEX_POINT('',#20666);
#6353=VERTEX_POINT('',#20668);
#6354=VERTEX_POINT('',#20672);
#6355=VERTEX_POINT('',#20674);
#6356=VERTEX_POINT('',#20678);
#6357=VERTEX_POINT('',#20680);
#6358=VERTEX_POINT('',#20684);
#6359=VERTEX_POINT('',#20686);
#6360=VERTEX_POINT('',#20690);
#6361=VERTEX_POINT('',#20692);
#6362=VERTEX_POINT('',#20696);
#6363=VERTEX_POINT('',#20698);
#6364=VERTEX_POINT('',#20702);
#6365=VERTEX_POINT('',#20704);
#6366=VERTEX_POINT('',#20708);
#6367=VERTEX_POINT('',#20710);
#6368=VERTEX_POINT('',#20714);
#6369=VERTEX_POINT('',#20716);
#6370=VERTEX_POINT('',#20720);
#6371=VERTEX_POINT('',#20722);
#6372=VERTEX_POINT('',#20726);
#6373=VERTEX_POINT('',#20728);
#6374=VERTEX_POINT('',#20732);
#6375=VERTEX_POINT('',#20734);
#6376=VERTEX_POINT('',#20738);
#6377=VERTEX_POINT('',#20740);
#6378=VERTEX_POINT('',#20744);
#6379=VERTEX_POINT('',#20746);
#6380=VERTEX_POINT('',#20750);
#6381=VERTEX_POINT('',#20752);
#6382=VERTEX_POINT('',#20756);
#6383=VERTEX_POINT('',#20758);
#6384=VERTEX_POINT('',#20767);
#6385=VERTEX_POINT('',#20770);
#6386=VERTEX_POINT('',#20777);
#6387=VERTEX_POINT('',#20778);
#6388=VERTEX_POINT('',#20782);
#6389=VERTEX_POINT('',#20793);
#6390=VERTEX_POINT('',#20795);
#6391=VERTEX_POINT('',#20802);
#6392=VERTEX_POINT('',#20804);
#6393=VERTEX_POINT('',#20850);
#6394=VERTEX_POINT('',#20852);
#6395=VERTEX_POINT('',#20856);
#6396=VERTEX_POINT('',#20858);
#6397=VERTEX_POINT('',#20863);
#6398=VERTEX_POINT('',#20865);
#6399=VERTEX_POINT('',#20872);
#6400=VERTEX_POINT('',#20874);
#6401=VERTEX_POINT('',#20881);
#6402=VERTEX_POINT('',#20883);
#6403=VERTEX_POINT('',#20890);
#6404=VERTEX_POINT('',#20891);
#6405=VERTEX_POINT('',#20928);
#6406=VERTEX_POINT('',#20930);
#6407=VERTEX_POINT('',#20968);
#6408=VERTEX_POINT('',#20969);
#6409=VERTEX_POINT('',#20971);
#6410=VERTEX_POINT('',#20973);
#6411=VERTEX_POINT('',#20977);
#6412=VERTEX_POINT('',#20978);
#6413=VERTEX_POINT('',#20980);
#6414=VERTEX_POINT('',#20982);
#6415=VERTEX_POINT('',#20986);
#6416=VERTEX_POINT('',#20988);
#6417=VERTEX_POINT('',#20992);
#6418=VERTEX_POINT('',#20994);
#6419=VERTEX_POINT('',#21007);
#6420=VERTEX_POINT('',#21008);
#6421=VERTEX_POINT('',#21010);
#6422=VERTEX_POINT('',#21012);
#6423=VERTEX_POINT('',#21016);
#6424=VERTEX_POINT('',#21018);
#6425=VERTEX_POINT('',#21022);
#6426=VERTEX_POINT('',#21024);
#6427=VERTEX_POINT('',#21028);
#6428=VERTEX_POINT('',#21030);
#6429=VERTEX_POINT('',#21034);
#6430=VERTEX_POINT('',#21036);
#6431=VERTEX_POINT('',#21044);
#6432=VERTEX_POINT('',#21047);
#6433=VERTEX_POINT('',#21051);
#6434=VERTEX_POINT('',#21055);
#6435=VERTEX_POINT('',#21068);
#6436=VERTEX_POINT('',#21070);
#6437=VERTEX_POINT('',#21075);
#6438=VERTEX_POINT('',#21077);
#6439=VERTEX_POINT('',#21082);
#6440=VERTEX_POINT('',#21083);
#6441=VERTEX_POINT('',#21085);
#6442=VERTEX_POINT('',#21087);
#6443=VERTEX_POINT('',#21091);
#6444=VERTEX_POINT('',#21093);
#6445=VERTEX_POINT('',#21097);
#6446=VERTEX_POINT('',#21101);
#6447=VERTEX_POINT('',#21107);
#6448=VERTEX_POINT('',#21108);
#6449=VERTEX_POINT('',#21110);
#6450=VERTEX_POINT('',#21112);
#6451=VERTEX_POINT('',#21116);
#6452=VERTEX_POINT('',#21118);
#6453=VERTEX_POINT('',#21122);
#6454=VERTEX_POINT('',#21126);
#6455=VERTEX_POINT('',#21132);
#6456=VERTEX_POINT('',#21134);
#6457=VERTEX_POINT('',#21141);
#6458=VERTEX_POINT('',#21143);
#6459=VERTEX_POINT('',#21147);
#6460=VERTEX_POINT('',#21149);
#6461=VERTEX_POINT('',#21156);
#6462=VERTEX_POINT('',#21158);
#6463=VERTEX_POINT('',#21162);
#6464=VERTEX_POINT('',#21164);
#6465=VERTEX_POINT('',#21171);
#6466=VERTEX_POINT('',#21173);
#6467=VERTEX_POINT('',#21177);
#6468=VERTEX_POINT('',#21179);
#6469=VERTEX_POINT('',#21186);
#6470=VERTEX_POINT('',#21188);
#6471=VERTEX_POINT('',#21192);
#6472=VERTEX_POINT('',#21194);
#6473=VERTEX_POINT('',#21201);
#6474=VERTEX_POINT('',#21202);
#6475=VERTEX_POINT('',#21204);
#6476=VERTEX_POINT('',#21206);
#6477=VERTEX_POINT('',#21210);
#6478=VERTEX_POINT('',#21212);
#6479=VERTEX_POINT('',#21216);
#6480=VERTEX_POINT('',#21218);
#6481=VERTEX_POINT('',#21228);
#6482=VERTEX_POINT('',#21229);
#6483=VERTEX_POINT('',#21231);
#6484=VERTEX_POINT('',#21233);
#6485=VERTEX_POINT('',#21237);
#6486=VERTEX_POINT('',#21239);
#6487=VERTEX_POINT('',#21243);
#6488=VERTEX_POINT('',#21245);
#6489=VERTEX_POINT('',#21255);
#6490=VERTEX_POINT('',#21257);
#6491=VERTEX_POINT('',#21261);
#6492=VERTEX_POINT('',#21262);
#6493=VERTEX_POINT('',#21264);
#6494=VERTEX_POINT('',#21266);
#6495=VERTEX_POINT('',#21270);
#6496=VERTEX_POINT('',#21272);
#6497=VERTEX_POINT('',#21276);
#6498=VERTEX_POINT('',#21278);
#6499=VERTEX_POINT('',#21282);
#6500=VERTEX_POINT('',#21288);
#6501=VERTEX_POINT('',#21289);
#6502=VERTEX_POINT('',#21291);
#6503=VERTEX_POINT('',#21293);
#6504=VERTEX_POINT('',#21297);
#6505=VERTEX_POINT('',#21299);
#6506=VERTEX_POINT('',#21303);
#6507=VERTEX_POINT('',#21307);
#6508=VERTEX_POINT('',#21313);
#6509=VERTEX_POINT('',#21319);
#6510=VERTEX_POINT('',#21321);
#6511=VERTEX_POINT('',#21325);
#6512=VERTEX_POINT('',#21327);
#6513=VERTEX_POINT('',#21334);
#6514=VERTEX_POINT('',#21336);
#6515=VERTEX_POINT('',#21340);
#6516=VERTEX_POINT('',#21342);
#6517=VERTEX_POINT('',#21349);
#6518=VERTEX_POINT('',#21351);
#6519=VERTEX_POINT('',#21355);
#6520=VERTEX_POINT('',#21357);
#6521=VERTEX_POINT('',#21364);
#6522=VERTEX_POINT('',#21365);
#6523=VERTEX_POINT('',#21367);
#6524=VERTEX_POINT('',#21369);
#6525=VERTEX_POINT('',#21373);
#6526=VERTEX_POINT('',#21375);
#6527=VERTEX_POINT('',#21379);
#6528=VERTEX_POINT('',#21381);
#6529=VERTEX_POINT('',#21385);
#6530=VERTEX_POINT('',#21386);
#6531=VERTEX_POINT('',#21388);
#6532=VERTEX_POINT('',#21459);
#6533=VERTEX_POINT('',#21461);
#6534=VERTEX_POINT('',#21532);
#6535=VERTEX_POINT('',#21534);
#6536=VERTEX_POINT('',#21605);
#6537=VERTEX_POINT('',#21607);
#6538=VERTEX_POINT('',#21678);
#6539=VERTEX_POINT('',#21680);
#6540=VERTEX_POINT('',#21751);
#6541=VERTEX_POINT('',#21753);
#6542=VERTEX_POINT('',#21824);
#6543=VERTEX_POINT('',#21826);
#6544=VERTEX_POINT('',#21897);
#6545=VERTEX_POINT('',#21899);
#6546=VERTEX_POINT('',#21970);
#6547=VERTEX_POINT('',#21972);
#6548=VERTEX_POINT('',#22043);
#6549=VERTEX_POINT('',#22045);
#6550=VERTEX_POINT('',#22116);
#6551=VERTEX_POINT('',#22118);
#6552=VERTEX_POINT('',#22189);
#6553=VERTEX_POINT('',#22191);
#6554=VERTEX_POINT('',#22262);
#6555=VERTEX_POINT('',#22264);
#6556=VERTEX_POINT('',#22335);
#6557=VERTEX_POINT('',#22337);
#6558=VERTEX_POINT('',#22408);
#6559=VERTEX_POINT('',#22410);
#6560=VERTEX_POINT('',#22481);
#6561=VERTEX_POINT('',#22483);
#6562=VERTEX_POINT('',#22554);
#6563=VERTEX_POINT('',#22556);
#6564=VERTEX_POINT('',#22627);
#6565=VERTEX_POINT('',#22629);
#6566=VERTEX_POINT('',#22700);
#6567=VERTEX_POINT('',#22702);
#6568=VERTEX_POINT('',#22773);
#6569=VERTEX_POINT('',#22775);
#6570=VERTEX_POINT('',#22846);
#6571=VERTEX_POINT('',#22848);
#6572=VERTEX_POINT('',#22919);
#6573=VERTEX_POINT('',#22921);
#6574=VERTEX_POINT('',#22992);
#6575=VERTEX_POINT('',#22994);
#6576=VERTEX_POINT('',#23065);
#6577=VERTEX_POINT('',#23067);
#6578=VERTEX_POINT('',#23138);
#6579=VERTEX_POINT('',#23140);
#6580=VERTEX_POINT('',#23211);
#6581=VERTEX_POINT('',#23213);
#6582=VERTEX_POINT('',#23284);
#6583=VERTEX_POINT('',#23286);
#6584=VERTEX_POINT('',#23357);
#6585=VERTEX_POINT('',#23359);
#6586=VERTEX_POINT('',#23430);
#6587=VERTEX_POINT('',#23432);
#6588=VERTEX_POINT('',#23503);
#6589=VERTEX_POINT('',#23505);
#6590=VERTEX_POINT('',#23576);
#6591=VERTEX_POINT('',#23578);
#6592=VERTEX_POINT('',#23649);
#6593=VERTEX_POINT('',#23651);
#6594=VERTEX_POINT('',#23722);
#6595=VERTEX_POINT('',#23724);
#6596=VERTEX_POINT('',#23795);
#6597=VERTEX_POINT('',#23797);
#6598=VERTEX_POINT('',#23868);
#6599=VERTEX_POINT('',#23870);
#6600=VERTEX_POINT('',#23941);
#6601=VERTEX_POINT('',#23943);
#6602=VERTEX_POINT('',#24014);
#6603=VERTEX_POINT('',#24016);
#6604=VERTEX_POINT('',#24087);
#6605=VERTEX_POINT('',#24089);
#6606=VERTEX_POINT('',#24160);
#6607=VERTEX_POINT('',#24162);
#6608=VERTEX_POINT('',#24233);
#6609=VERTEX_POINT('',#24309);
#6610=VERTEX_POINT('',#24311);
#6611=VERTEX_POINT('',#24455);
#6612=VERTEX_POINT('',#24457);
#6613=VERTEX_POINT('',#24530);
#6614=VERTEX_POINT('',#24673);
#6615=VERTEX_POINT('',#24746);
#6616=VERTEX_POINT('',#24889);
#6617=VERTEX_POINT('',#24962);
#6618=VERTEX_POINT('',#25105);
#6619=VERTEX_POINT('',#25178);
#6620=VERTEX_POINT('',#25321);
#6621=VERTEX_POINT('',#25394);
#6622=VERTEX_POINT('',#25537);
#6623=VERTEX_POINT('',#25610);
#6624=VERTEX_POINT('',#25753);
#6625=VERTEX_POINT('',#25826);
#6626=VERTEX_POINT('',#25969);
#6627=VERTEX_POINT('',#26042);
#6628=VERTEX_POINT('',#26185);
#6629=VERTEX_POINT('',#26258);
#6630=VERTEX_POINT('',#26401);
#6631=VERTEX_POINT('',#26474);
#6632=VERTEX_POINT('',#26617);
#6633=VERTEX_POINT('',#26690);
#6634=VERTEX_POINT('',#26833);
#6635=VERTEX_POINT('',#26906);
#6636=VERTEX_POINT('',#27049);
#6637=VERTEX_POINT('',#27122);
#6638=VERTEX_POINT('',#27265);
#6639=VERTEX_POINT('',#27338);
#6640=VERTEX_POINT('',#27481);
#6641=VERTEX_POINT('',#27554);
#6642=VERTEX_POINT('',#27697);
#6643=VERTEX_POINT('',#27770);
#6644=VERTEX_POINT('',#27913);
#6645=VERTEX_POINT('',#27986);
#6646=VERTEX_POINT('',#28129);
#6647=VERTEX_POINT('',#28202);
#6648=VERTEX_POINT('',#28345);
#6649=VERTEX_POINT('',#28418);
#6650=VERTEX_POINT('',#28561);
#6651=VERTEX_POINT('',#28634);
#6652=VERTEX_POINT('',#28777);
#6653=VERTEX_POINT('',#28850);
#6654=VERTEX_POINT('',#28993);
#6655=VERTEX_POINT('',#29066);
#6656=VERTEX_POINT('',#29209);
#6657=VERTEX_POINT('',#29282);
#6658=VERTEX_POINT('',#29425);
#6659=VERTEX_POINT('',#29498);
#6660=VERTEX_POINT('',#29641);
#6661=VERTEX_POINT('',#29714);
#6662=VERTEX_POINT('',#29857);
#6663=VERTEX_POINT('',#29930);
#6664=VERTEX_POINT('',#30073);
#6665=VERTEX_POINT('',#30146);
#6666=VERTEX_POINT('',#30289);
#6667=VERTEX_POINT('',#30362);
#6668=VERTEX_POINT('',#30505);
#6669=VERTEX_POINT('',#30578);
#6670=VERTEX_POINT('',#30721);
#6671=VERTEX_POINT('',#30794);
#6672=VERTEX_POINT('',#30937);
#6673=VERTEX_POINT('',#31010);
#6674=VERTEX_POINT('',#31153);
#6675=VERTEX_POINT('',#31226);
#6676=VERTEX_POINT('',#31369);
#6677=VERTEX_POINT('',#31442);
#6678=VERTEX_POINT('',#31585);
#6679=VERTEX_POINT('',#31658);
#6680=VERTEX_POINT('',#31801);
#6681=VERTEX_POINT('',#31874);
#6682=VERTEX_POINT('',#32017);
#6683=VERTEX_POINT('',#32090);
#6684=VERTEX_POINT('',#32233);
#6685=VERTEX_POINT('',#32306);
#6686=VERTEX_POINT('',#32449);
#6687=VERTEX_POINT('',#32522);
#6688=VERTEX_POINT('',#32665);
#6689=VERTEX_POINT('',#32738);
#6690=VERTEX_POINT('',#32881);
#6691=VERTEX_POINT('',#32958);
#6692=VERTEX_POINT('',#32960);
#6693=VERTEX_POINT('',#32964);
#6694=VERTEX_POINT('',#32966);
#6695=VERTEX_POINT('',#32973);
#6696=VERTEX_POINT('',#32976);
#6697=VERTEX_POINT('',#32980);
#6698=VERTEX_POINT('',#32984);
#6699=VERTEX_POINT('',#32988);
#6700=VERTEX_POINT('',#32991);
#6701=VERTEX_POINT('',#32995);
#6702=VERTEX_POINT('',#32999);
#6703=VERTEX_POINT('',#33004);
#6704=VERTEX_POINT('',#33005);
#6705=VERTEX_POINT('',#33007);
#6706=VERTEX_POINT('',#33009);
#6707=VERTEX_POINT('',#33013);
#6708=VERTEX_POINT('',#33015);
#6709=VERTEX_POINT('',#33019);
#6710=VERTEX_POINT('',#33021);
#6711=VERTEX_POINT('',#33025);
#6712=VERTEX_POINT('',#33027);
#6713=VERTEX_POINT('',#33031);
#6714=VERTEX_POINT('',#33033);
#6715=VERTEX_POINT('',#33043);
#6716=VERTEX_POINT('',#33046);
#6717=VERTEX_POINT('',#33050);
#6718=VERTEX_POINT('',#33054);
#6719=VERTEX_POINT('',#33058);
#6720=VERTEX_POINT('',#33061);
#6721=VERTEX_POINT('',#33065);
#6722=VERTEX_POINT('',#33069);
#6723=VERTEX_POINT('',#33074);
#6724=VERTEX_POINT('',#33075);
#6725=VERTEX_POINT('',#33077);
#6726=VERTEX_POINT('',#33079);
#6727=VERTEX_POINT('',#33083);
#6728=VERTEX_POINT('',#33085);
#6729=VERTEX_POINT('',#33089);
#6730=VERTEX_POINT('',#33091);
#6731=VERTEX_POINT('',#33095);
#6732=VERTEX_POINT('',#33097);
#6733=VERTEX_POINT('',#33101);
#6734=VERTEX_POINT('',#33103);
#6735=VERTEX_POINT('',#33178);
#6736=VERTEX_POINT('',#33180);
#6737=VERTEX_POINT('',#33184);
#6738=VERTEX_POINT('',#33186);
#6739=EDGE_CURVE('',#5613,#5613,#5214,.T.);
#6740=EDGE_CURVE('',#5613,#5614,#2884,.T.);
#6741=EDGE_CURVE('',#5614,#5614,#5215,.T.);
#6742=EDGE_CURVE('',#5615,#5615,#5216,.T.);
#6743=EDGE_CURVE('',#5615,#5616,#2885,.T.);
#6744=EDGE_CURVE('',#5616,#5616,#5217,.T.);
#6745=EDGE_CURVE('',#5617,#5617,#5218,.T.);
#6746=EDGE_CURVE('',#5617,#5618,#2886,.T.);
#6747=EDGE_CURVE('',#5618,#5618,#5219,.T.);
#6748=EDGE_CURVE('',#5619,#5619,#5220,.T.);
#6749=EDGE_CURVE('',#5619,#5620,#2887,.T.);
#6750=EDGE_CURVE('',#5620,#5620,#5221,.T.);
#6751=EDGE_CURVE('',#5621,#5621,#5222,.T.);
#6752=EDGE_CURVE('',#5621,#5622,#2888,.T.);
#6753=EDGE_CURVE('',#5622,#5622,#5223,.T.);
#6754=EDGE_CURVE('',#5623,#5623,#5224,.T.);
#6755=EDGE_CURVE('',#5623,#5624,#2889,.T.);
#6756=EDGE_CURVE('',#5624,#5624,#5225,.T.);
#6757=EDGE_CURVE('',#5625,#5626,#2890,.T.);
#6758=EDGE_CURVE('',#5626,#5627,#2891,.T.);
#6759=EDGE_CURVE('',#5628,#5627,#2892,.T.);
#6760=EDGE_CURVE('',#5625,#5628,#2893,.T.);
#6761=EDGE_CURVE('',#5629,#5625,#2894,.T.);
#6762=EDGE_CURVE('',#5630,#5628,#2895,.T.);
#6763=EDGE_CURVE('',#5629,#5630,#2896,.T.);
#6764=EDGE_CURVE('',#5631,#5629,#2897,.T.);
#6765=EDGE_CURVE('',#5632,#5630,#2898,.T.);
#6766=EDGE_CURVE('',#5631,#5632,#2899,.T.);
#6767=EDGE_CURVE('',#5626,#5631,#2900,.T.);
#6768=EDGE_CURVE('',#5627,#5632,#2901,.T.);
#6769=EDGE_CURVE('',#5633,#5634,#2902,.T.);
#6770=EDGE_CURVE('',#5634,#5635,#2903,.T.);
#6771=EDGE_CURVE('',#5636,#5635,#2904,.T.);
#6772=EDGE_CURVE('',#5633,#5636,#2905,.T.);
#6773=EDGE_CURVE('',#5637,#5633,#2906,.T.);
#6774=EDGE_CURVE('',#5638,#5636,#2907,.T.);
#6775=EDGE_CURVE('',#5637,#5638,#2908,.T.);
#6776=EDGE_CURVE('',#5639,#5637,#2909,.T.);
#6777=EDGE_CURVE('',#5640,#5638,#2910,.T.);
#6778=EDGE_CURVE('',#5639,#5640,#2911,.T.);
#6779=EDGE_CURVE('',#5634,#5639,#2912,.T.);
#6780=EDGE_CURVE('',#5635,#5640,#2913,.T.);
#6781=EDGE_CURVE('',#5641,#5642,#2914,.T.);
#6782=EDGE_CURVE('',#5642,#5643,#2915,.T.);
#6783=EDGE_CURVE('',#5644,#5643,#2916,.T.);
#6784=EDGE_CURVE('',#5641,#5644,#2917,.T.);
#6785=EDGE_CURVE('',#5645,#5641,#2918,.T.);
#6786=EDGE_CURVE('',#5646,#5644,#2919,.T.);
#6787=EDGE_CURVE('',#5645,#5646,#2920,.T.);
#6788=EDGE_CURVE('',#5647,#5645,#2921,.T.);
#6789=EDGE_CURVE('',#5648,#5646,#2922,.T.);
#6790=EDGE_CURVE('',#5647,#5648,#2923,.T.);
#6791=EDGE_CURVE('',#5642,#5647,#2924,.T.);
#6792=EDGE_CURVE('',#5643,#5648,#2925,.T.);
#6793=EDGE_CURVE('',#5649,#5649,#5226,.T.);
#6794=EDGE_CURVE('',#5649,#5650,#2926,.T.);
#6795=EDGE_CURVE('',#5650,#5650,#5227,.T.);
#6796=EDGE_CURVE('',#5651,#5651,#5228,.T.);
#6797=EDGE_CURVE('',#5651,#5652,#2927,.T.);
#6798=EDGE_CURVE('',#5652,#5652,#5229,.T.);
#6799=EDGE_CURVE('',#5653,#5654,#2928,.T.);
#6800=EDGE_CURVE('',#5655,#5653,#2929,.T.);
#6801=EDGE_CURVE('',#5656,#5655,#2930,.T.);
#6802=EDGE_CURVE('',#5654,#5656,#2931,.T.);
#6803=EDGE_CURVE('',#5657,#5658,#2932,.T.);
#6804=EDGE_CURVE('',#5659,#5657,#2933,.T.);
#6805=EDGE_CURVE('',#5660,#5659,#2934,.T.);
#6806=EDGE_CURVE('',#5658,#5660,#2935,.T.);
#6807=EDGE_CURVE('',#5661,#5653,#5230,.T.);
#6808=EDGE_CURVE('',#5662,#5661,#2936,.T.);
#6809=EDGE_CURVE('',#5663,#5662,#2937,.T.);
#6810=EDGE_CURVE('',#5664,#5663,#2938,.T.);
#6811=EDGE_CURVE('',#5658,#5664,#5231,.T.);
#6812=EDGE_CURVE('',#5660,#5655,#5232,.T.);
#6813=EDGE_CURVE('',#5656,#5659,#5233,.T.);
#6814=EDGE_CURVE('',#5664,#5665,#2939,.T.);
#6815=EDGE_CURVE('',#5657,#5665,#5234,.T.);
#6816=EDGE_CURVE('',#5666,#5654,#5235,.T.);
#6817=EDGE_CURVE('',#5661,#5666,#2940,.T.);
#6818=EDGE_CURVE('',#5665,#5667,#2941,.T.);
#6819=EDGE_CURVE('',#5668,#5667,#2942,.T.);
#6820=EDGE_CURVE('',#5668,#5666,#2943,.T.);
#6821=EDGE_CURVE('',#5667,#5663,#2944,.T.);
#6822=EDGE_CURVE('',#5662,#5668,#2945,.T.);
#6823=EDGE_CURVE('',#5669,#5669,#5236,.T.);
#6824=EDGE_CURVE('',#5669,#5670,#2946,.T.);
#6825=EDGE_CURVE('',#5670,#5670,#5237,.T.);
#6826=EDGE_CURVE('',#5671,#5671,#5238,.T.);
#6827=EDGE_CURVE('',#5671,#5672,#2947,.T.);
#6828=EDGE_CURVE('',#5672,#5672,#5239,.T.);
#6829=EDGE_CURVE('',#5673,#5674,#2948,.T.);
#6830=EDGE_CURVE('',#5675,#5673,#2949,.T.);
#6831=EDGE_CURVE('',#5676,#5675,#2950,.T.);
#6832=EDGE_CURVE('',#5674,#5676,#2951,.T.);
#6833=EDGE_CURVE('',#5677,#5678,#2952,.T.);
#6834=EDGE_CURVE('',#5679,#5677,#2953,.T.);
#6835=EDGE_CURVE('',#5680,#5679,#2954,.T.);
#6836=EDGE_CURVE('',#5678,#5680,#2955,.T.);
#6837=EDGE_CURVE('',#5681,#5673,#5240,.T.);
#6838=EDGE_CURVE('',#5682,#5681,#2956,.T.);
#6839=EDGE_CURVE('',#5683,#5682,#2957,.T.);
#6840=EDGE_CURVE('',#5684,#5683,#2958,.T.);
#6841=EDGE_CURVE('',#5685,#5684,#2959,.T.);
#6842=EDGE_CURVE('',#5685,#5686,#5241,.T.);
#6843=EDGE_CURVE('',#5686,#5687,#5242,.T.);
#6844=EDGE_CURVE('',#5688,#5687,#2960,.T.);
#6845=EDGE_CURVE('',#5689,#5688,#2961,.T.);
#6846=EDGE_CURVE('',#5690,#5689,#2962,.T.);
#6847=EDGE_CURVE('',#5691,#5690,#2963,.T.);
#6848=EDGE_CURVE('',#5678,#5691,#5243,.T.);
#6849=EDGE_CURVE('',#5680,#5675,#5244,.T.);
#6850=EDGE_CURVE('',#5676,#5679,#5245,.T.);
#6851=EDGE_CURVE('',#5691,#5692,#2964,.T.);
#6852=EDGE_CURVE('',#5677,#5692,#5246,.T.);
#6853=EDGE_CURVE('',#5693,#5674,#5247,.T.);
#6854=EDGE_CURVE('',#5681,#5693,#2965,.T.);
#6855=EDGE_CURVE('',#5692,#5694,#2966,.T.);
#6856=EDGE_CURVE('',#5695,#5694,#2967,.T.);
#6857=EDGE_CURVE('',#5695,#5693,#2968,.T.);
#6858=EDGE_CURVE('',#5682,#5695,#2969,.T.);
#6859=EDGE_CURVE('',#5694,#5690,#2970,.T.);
#6860=EDGE_CURVE('',#5689,#5696,#2971,.T.);
#6861=EDGE_CURVE('',#5697,#5696,#2972,.T.);
#6862=EDGE_CURVE('',#5683,#5697,#2973,.T.);
#6863=EDGE_CURVE('',#5698,#5699,#2974,.T.);
#6864=EDGE_CURVE('',#5698,#5699,#5248,.T.);
#6865=EDGE_CURVE('',#5700,#5698,#491,.T.);
#6866=EDGE_CURVE('',#5701,#5700,#5249,.T.);
#6867=EDGE_CURVE('',#5702,#5701,#492,.T.);
#6868=EDGE_CURVE('',#5702,#5703,#2975,.T.);
#6869=EDGE_CURVE('',#5704,#5703,#493,.T.);
#6870=EDGE_CURVE('',#5703,#5704,#494,.T.);
#6871=EDGE_CURVE('',#5699,#5702,#495,.T.);
#6872=EDGE_CURVE('',#5701,#5700,#2976,.T.);
#6873=EDGE_CURVE('',#5687,#5685,#2977,.T.);
#6874=EDGE_CURVE('',#5687,#5685,#5250,.T.);
#6875=EDGE_CURVE('',#5705,#5705,#5251,.T.);
#6876=EDGE_CURVE('',#5705,#5706,#2978,.T.);
#6877=EDGE_CURVE('',#5706,#5706,#5252,.T.);
#6878=EDGE_CURVE('',#5686,#5707,#2979,.T.);
#6879=EDGE_CURVE('',#5707,#5707,#5253,.T.);
#6880=EDGE_CURVE('',#5708,#5697,#2980,.T.);
#6881=EDGE_CURVE('',#5684,#5708,#2981,.T.);
#6882=EDGE_CURVE('',#5709,#5708,#2982,.T.);
#6883=EDGE_CURVE('',#5688,#5709,#2983,.T.);
#6884=EDGE_CURVE('',#5696,#5709,#2984,.T.);
#6885=EDGE_CURVE('',#5710,#5711,#2985,.T.);
#6886=EDGE_CURVE('',#5710,#5712,#5254,.T.);
#6887=EDGE_CURVE('',#5713,#5712,#2986,.T.);
#6888=EDGE_CURVE('',#5711,#5713,#5255,.T.);
#6889=EDGE_CURVE('',#5712,#5710,#5256,.T.);
#6890=EDGE_CURVE('',#5714,#5715,#2987,.T.);
#6891=EDGE_CURVE('',#5714,#5716,#5257,.T.);
#6892=EDGE_CURVE('',#5717,#5716,#2988,.T.);
#6893=EDGE_CURVE('',#5715,#5717,#5258,.T.);
#6894=EDGE_CURVE('',#5716,#5714,#5259,.T.);
#6895=EDGE_CURVE('',#5718,#5718,#5260,.T.);
#6896=EDGE_CURVE('',#5713,#5719,#5261,.T.);
#6897=EDGE_CURVE('',#5719,#5715,#5262,.T.);
#6898=EDGE_CURVE('',#5717,#5711,#5263,.T.);
#6899=EDGE_CURVE('',#5720,#5720,#5264,.T.);
#6900=EDGE_CURVE('',#5721,#5721,#5265,.T.);
#6901=EDGE_CURVE('',#5722,#5723,#2989,.T.);
#6902=EDGE_CURVE('',#5722,#5723,#5266,.T.);
#6903=EDGE_CURVE('',#5724,#5722,#496,.T.);
#6904=EDGE_CURVE('',#5725,#5724,#5267,.T.);
#6905=EDGE_CURVE('',#5726,#5725,#497,.T.);
#6906=EDGE_CURVE('',#5726,#5727,#2990,.T.);
#6907=EDGE_CURVE('',#5728,#5727,#498,.T.);
#6908=EDGE_CURVE('',#5727,#5728,#499,.T.);
#6909=EDGE_CURVE('',#5723,#5726,#500,.T.);
#6910=EDGE_CURVE('',#5725,#5724,#2991,.T.);
#6911=EDGE_CURVE('',#5729,#5729,#5268,.T.);
#6912=EDGE_CURVE('',#5729,#5720,#2992,.T.);
#6913=EDGE_CURVE('',#5730,#5730,#5269,.T.);
#6914=EDGE_CURVE('',#5730,#5721,#2993,.T.);
#6915=EDGE_CURVE('',#5731,#5731,#5270,.T.);
#6916=EDGE_CURVE('',#5731,#5719,#2994,.T.);
#6917=EDGE_CURVE('',#5732,#5732,#5271,.T.);
#6918=EDGE_CURVE('',#5732,#5733,#2995,.T.);
#6919=EDGE_CURVE('',#5733,#5733,#5272,.T.);
#6920=EDGE_CURVE('',#5718,#5734,#2996,.T.);
#6921=EDGE_CURVE('',#5734,#5734,#5273,.T.);
#6922=EDGE_CURVE('',#5735,#5736,#2997,.T.);
#6923=EDGE_CURVE('',#5735,#5737,#2998,.T.);
#6924=EDGE_CURVE('',#5738,#5737,#2999,.T.);
#6925=EDGE_CURVE('',#5736,#5738,#3000,.T.);
#6926=EDGE_CURVE('',#5739,#5740,#3001,.T.);
#6927=EDGE_CURVE('',#5741,#5739,#3002,.T.);
#6928=EDGE_CURVE('',#5742,#5741,#3003,.T.);
#6929=EDGE_CURVE('',#5740,#5742,#3004,.T.);
#6930=EDGE_CURVE('',#5743,#5739,#3005,.T.);
#6931=EDGE_CURVE('',#5744,#5743,#3006,.T.);
#6932=EDGE_CURVE('',#5745,#5744,#3007,.T.);
#6933=EDGE_CURVE('',#5746,#5745,#3008,.T.);
#6934=EDGE_CURVE('',#5741,#5746,#3009,.T.);
#6935=EDGE_CURVE('',#5747,#5735,#3010,.T.);
#6936=EDGE_CURVE('',#5748,#5747,#3011,.T.);
#6937=EDGE_CURVE('',#5749,#5748,#3012,.T.);
#6938=EDGE_CURVE('',#5750,#5749,#3013,.T.);
#6939=EDGE_CURVE('',#5737,#5750,#3014,.T.);
#6940=EDGE_CURVE('',#5747,#5746,#5274,.T.);
#6941=EDGE_CURVE('',#5742,#5736,#5275,.T.);
#6942=EDGE_CURVE('',#5740,#5738,#5276,.T.);
#6943=EDGE_CURVE('',#5748,#5745,#5277,.T.);
#6944=EDGE_CURVE('',#5749,#5744,#5278,.T.);
#6945=EDGE_CURVE('',#5750,#5743,#5279,.T.);
#6946=EDGE_CURVE('',#5751,#5751,#5280,.T.);
#6947=EDGE_CURVE('',#5751,#5752,#3015,.T.);
#6948=EDGE_CURVE('',#5752,#5752,#5281,.T.);
#6949=EDGE_CURVE('',#5753,#5753,#5282,.T.);
#6950=EDGE_CURVE('',#5753,#5754,#3016,.T.);
#6951=EDGE_CURVE('',#5754,#5754,#5283,.T.);
#6952=EDGE_CURVE('',#5755,#5756,#3017,.T.);
#6953=EDGE_CURVE('',#5755,#5757,#3018,.T.);
#6954=EDGE_CURVE('',#5758,#5757,#3019,.T.);
#6955=EDGE_CURVE('',#5756,#5758,#3020,.T.);
#6956=EDGE_CURVE('',#5759,#5760,#3021,.T.);
#6957=EDGE_CURVE('',#5761,#5759,#3022,.T.);
#6958=EDGE_CURVE('',#5762,#5761,#3023,.T.);
#6959=EDGE_CURVE('',#5760,#5762,#3024,.T.);
#6960=EDGE_CURVE('',#5763,#5759,#3025,.T.);
#6961=EDGE_CURVE('',#5764,#5763,#3026,.T.);
#6962=EDGE_CURVE('',#5761,#5764,#3027,.T.);
#6963=EDGE_CURVE('',#5765,#5755,#3028,.T.);
#6964=EDGE_CURVE('',#5766,#5765,#3029,.T.);
#6965=EDGE_CURVE('',#5757,#5766,#3030,.T.);
#6966=EDGE_CURVE('',#5767,#5758,#3031,.T.);
#6967=EDGE_CURVE('',#5768,#5767,#3032,.T.);
#6968=EDGE_CURVE('',#5768,#5756,#3033,.T.);
#6969=EDGE_CURVE('',#5762,#5769,#3034,.T.);
#6970=EDGE_CURVE('',#5769,#5770,#3035,.T.);
#6971=EDGE_CURVE('',#5760,#5770,#3036,.T.);
#6972=EDGE_CURVE('',#5766,#5763,#5284,.T.);
#6973=EDGE_CURVE('',#5770,#5771,#3037,.T.);
#6974=EDGE_CURVE('',#5771,#5772,#3038,.T.);
#6975=EDGE_CURVE('',#5772,#5767,#3039,.T.);
#6976=EDGE_CURVE('',#5764,#5765,#5285,.T.);
#6977=EDGE_CURVE('',#5773,#5768,#3040,.T.);
#6978=EDGE_CURVE('',#5773,#5772,#3041,.T.);
#6979=EDGE_CURVE('',#5774,#5773,#3042,.T.);
#6980=EDGE_CURVE('',#5774,#5771,#3043,.T.);
#6981=EDGE_CURVE('',#5769,#5774,#3044,.T.);
#6982=EDGE_CURVE('',#5775,#5776,#3045,.T.);
#6983=EDGE_CURVE('',#5775,#5777,#3046,.T.);
#6984=EDGE_CURVE('',#5778,#5777,#3047,.T.);
#6985=EDGE_CURVE('',#5776,#5778,#3048,.T.);
#6986=EDGE_CURVE('',#5779,#5780,#3049,.T.);
#6987=EDGE_CURVE('',#5781,#5779,#3050,.T.);
#6988=EDGE_CURVE('',#5782,#5781,#3051,.T.);
#6989=EDGE_CURVE('',#5780,#5782,#3052,.T.);
#6990=EDGE_CURVE('',#5783,#5779,#3053,.T.);
#6991=EDGE_CURVE('',#5784,#5783,#3054,.T.);
#6992=EDGE_CURVE('',#5785,#5784,#3055,.T.);
#6993=EDGE_CURVE('',#5786,#5785,#3056,.T.);
#6994=EDGE_CURVE('',#5781,#5786,#3057,.T.);
#6995=EDGE_CURVE('',#5787,#5775,#3058,.T.);
#6996=EDGE_CURVE('',#5788,#5787,#3059,.T.);
#6997=EDGE_CURVE('',#5789,#5788,#3060,.T.);
#6998=EDGE_CURVE('',#5790,#5789,#3061,.T.);
#6999=EDGE_CURVE('',#5777,#5790,#3062,.T.);
#7000=EDGE_CURVE('',#5787,#5786,#5286,.T.);
#7001=EDGE_CURVE('',#5782,#5776,#5287,.T.);
#7002=EDGE_CURVE('',#5780,#5778,#5288,.T.);
#7003=EDGE_CURVE('',#5788,#5785,#5289,.T.);
#7004=EDGE_CURVE('',#5789,#5784,#5290,.T.);
#7005=EDGE_CURVE('',#5790,#5783,#5291,.T.);
#7006=EDGE_CURVE('',#5791,#5791,#5292,.T.);
#7007=EDGE_CURVE('',#5791,#5792,#3063,.T.);
#7008=EDGE_CURVE('',#5792,#5792,#5293,.T.);
#7009=EDGE_CURVE('',#5793,#5793,#5294,.T.);
#7010=EDGE_CURVE('',#5793,#5794,#3064,.T.);
#7011=EDGE_CURVE('',#5794,#5794,#5295,.T.);
#7012=EDGE_CURVE('',#5795,#5796,#3065,.T.);
#7013=EDGE_CURVE('',#5795,#5797,#3066,.T.);
#7014=EDGE_CURVE('',#5798,#5797,#3067,.T.);
#7015=EDGE_CURVE('',#5796,#5798,#3068,.T.);
#7016=EDGE_CURVE('',#5799,#5800,#3069,.T.);
#7017=EDGE_CURVE('',#5801,#5799,#3070,.T.);
#7018=EDGE_CURVE('',#5802,#5801,#3071,.T.);
#7019=EDGE_CURVE('',#5800,#5802,#3072,.T.);
#7020=EDGE_CURVE('',#5803,#5799,#3073,.T.);
#7021=EDGE_CURVE('',#5804,#5803,#3074,.T.);
#7022=EDGE_CURVE('',#5801,#5804,#3075,.T.);
#7023=EDGE_CURVE('',#5805,#5795,#3076,.T.);
#7024=EDGE_CURVE('',#5806,#5805,#3077,.T.);
#7025=EDGE_CURVE('',#5797,#5806,#3078,.T.);
#7026=EDGE_CURVE('',#5807,#5798,#3079,.T.);
#7027=EDGE_CURVE('',#5808,#5807,#3080,.T.);
#7028=EDGE_CURVE('',#5808,#5796,#3081,.T.);
#7029=EDGE_CURVE('',#5802,#5809,#3082,.T.);
#7030=EDGE_CURVE('',#5809,#5810,#3083,.T.);
#7031=EDGE_CURVE('',#5800,#5810,#3084,.T.);
#7032=EDGE_CURVE('',#5806,#5803,#5296,.T.);
#7033=EDGE_CURVE('',#5810,#5811,#3085,.T.);
#7034=EDGE_CURVE('',#5811,#5812,#3086,.T.);
#7035=EDGE_CURVE('',#5812,#5807,#3087,.T.);
#7036=EDGE_CURVE('',#5804,#5805,#5297,.T.);
#7037=EDGE_CURVE('',#5813,#5808,#3088,.T.);
#7038=EDGE_CURVE('',#5813,#5812,#3089,.T.);
#7039=EDGE_CURVE('',#5814,#5813,#3090,.T.);
#7040=EDGE_CURVE('',#5814,#5811,#3091,.T.);
#7041=EDGE_CURVE('',#5809,#5814,#3092,.T.);
#7042=EDGE_CURVE('',#5815,#5816,#3093,.T.);
#7043=EDGE_CURVE('',#5817,#5815,#3094,.T.);
#7044=EDGE_CURVE('',#5818,#5817,#3095,.T.);
#7045=EDGE_CURVE('',#5816,#5818,#3096,.T.);
#7046=EDGE_CURVE('',#5819,#5818,#3097,.T.);
#7047=EDGE_CURVE('',#5819,#5820,#3098,.T.);
#7048=EDGE_CURVE('',#5816,#5820,#3099,.T.);
#7049=EDGE_CURVE('',#5821,#5817,#3100,.T.);
#7050=EDGE_CURVE('',#5821,#5819,#3101,.T.);
#7051=EDGE_CURVE('',#5822,#5822,#5298,.T.);
#7052=EDGE_CURVE('',#5823,#5823,#5299,.T.);
#7053=EDGE_CURVE('',#5820,#5824,#3102,.T.);
#7054=EDGE_CURVE('',#5824,#5821,#3103,.T.);
#7055=EDGE_CURVE('',#5824,#5815,#3104,.T.);
#7056=EDGE_CURVE('',#5825,#5825,#5300,.T.);
#7057=EDGE_CURVE('',#5826,#5826,#5301,.T.);
#7058=EDGE_CURVE('',#5827,#5828,#3105,.T.);
#7059=EDGE_CURVE('',#5827,#5828,#5302,.T.);
#7060=EDGE_CURVE('',#5829,#5827,#501,.T.);
#7061=EDGE_CURVE('',#5830,#5829,#5303,.T.);
#7062=EDGE_CURVE('',#5831,#5830,#502,.T.);
#7063=EDGE_CURVE('',#5831,#5832,#3106,.T.);
#7064=EDGE_CURVE('',#5833,#5832,#503,.T.);
#7065=EDGE_CURVE('',#5832,#5833,#504,.T.);
#7066=EDGE_CURVE('',#5828,#5831,#505,.T.);
#7067=EDGE_CURVE('',#5830,#5829,#3107,.T.);
#7068=EDGE_CURVE('',#5822,#5826,#3108,.T.);
#7069=EDGE_CURVE('',#5834,#5834,#5304,.T.);
#7070=EDGE_CURVE('',#5834,#5825,#3109,.T.);
#7071=EDGE_CURVE('',#5823,#5835,#3110,.T.);
#7072=EDGE_CURVE('',#5835,#5835,#5305,.T.);
#7073=EDGE_CURVE('',#5836,#5836,#5306,.T.);
#7074=EDGE_CURVE('',#5836,#5837,#3111,.T.);
#7075=EDGE_CURVE('',#5837,#5837,#5307,.T.);
#7076=EDGE_CURVE('',#5838,#5838,#5308,.T.);
#7077=EDGE_CURVE('',#5838,#5839,#3112,.T.);
#7078=EDGE_CURVE('',#5839,#5839,#5309,.T.);
#7079=EDGE_CURVE('',#5840,#5840,#5310,.T.);
#7080=EDGE_CURVE('',#5840,#5841,#3113,.T.);
#7081=EDGE_CURVE('',#5841,#5841,#5311,.T.);
#7082=EDGE_CURVE('',#5842,#5842,#5312,.T.);
#7083=EDGE_CURVE('',#5842,#5843,#3114,.T.);
#7084=EDGE_CURVE('',#5843,#5843,#5313,.T.);
#7085=EDGE_CURVE('',#5844,#5844,#5314,.T.);
#7086=EDGE_CURVE('',#5844,#5845,#3115,.T.);
#7087=EDGE_CURVE('',#5845,#5845,#5315,.T.);
#7088=EDGE_CURVE('',#5846,#5846,#5316,.T.);
#7089=EDGE_CURVE('',#5846,#5847,#3116,.T.);
#7090=EDGE_CURVE('',#5847,#5847,#5317,.T.);
#7091=EDGE_CURVE('',#5848,#5848,#5318,.T.);
#7092=EDGE_CURVE('',#5848,#5849,#3117,.T.);
#7093=EDGE_CURVE('',#5849,#5849,#5319,.T.);
#7094=EDGE_CURVE('',#5850,#5851,#3118,.T.);
#7095=EDGE_CURVE('',#5852,#5850,#3119,.T.);
#7096=EDGE_CURVE('',#5852,#5853,#3120,.T.);
#7097=EDGE_CURVE('',#5851,#5853,#3121,.T.);
#7098=EDGE_CURVE('',#5854,#5855,#3122,.T.);
#7099=EDGE_CURVE('',#5856,#5854,#3123,.T.);
#7100=EDGE_CURVE('',#5857,#5856,#3124,.T.);
#7101=EDGE_CURVE('',#5855,#5857,#3125,.T.);
#7102=EDGE_CURVE('',#5857,#5858,#3126,.T.);
#7103=EDGE_CURVE('',#5859,#5856,#3127,.T.);
#7104=EDGE_CURVE('',#5858,#5859,#3128,.T.);
#7105=EDGE_CURVE('',#5860,#5852,#3129,.T.);
#7106=EDGE_CURVE('',#5860,#5861,#3130,.T.);
#7107=EDGE_CURVE('',#5853,#5861,#3131,.T.);
#7108=EDGE_CURVE('',#5850,#5862,#3132,.T.);
#7109=EDGE_CURVE('',#5863,#5862,#3133,.T.);
#7110=EDGE_CURVE('',#5855,#5863,#3134,.T.);
#7111=EDGE_CURVE('',#5858,#5860,#3135,.T.);
#7112=EDGE_CURVE('',#5851,#5864,#3136,.T.);
#7113=EDGE_CURVE('',#5862,#5864,#3137,.T.);
#7114=EDGE_CURVE('',#5854,#5865,#3138,.T.);
#7115=EDGE_CURVE('',#5864,#5865,#3139,.T.);
#7116=EDGE_CURVE('',#5861,#5859,#3140,.T.);
#7117=EDGE_CURVE('',#5865,#5863,#3141,.T.);
#7118=EDGE_CURVE('',#5866,#5866,#5320,.T.);
#7119=EDGE_CURVE('',#5866,#5867,#3142,.T.);
#7120=EDGE_CURVE('',#5867,#5867,#5321,.T.);
#7121=EDGE_CURVE('',#5868,#5868,#5322,.T.);
#7122=EDGE_CURVE('',#5868,#5869,#3143,.T.);
#7123=EDGE_CURVE('',#5869,#5869,#5323,.T.);
#7124=EDGE_CURVE('',#5870,#5870,#5324,.T.);
#7125=EDGE_CURVE('',#5870,#5871,#3144,.T.);
#7126=EDGE_CURVE('',#5871,#5871,#5325,.T.);
#7127=EDGE_CURVE('',#5872,#5872,#5326,.T.);
#7128=EDGE_CURVE('',#5872,#5873,#3145,.T.);
#7129=EDGE_CURVE('',#5873,#5873,#5327,.T.);
#7130=EDGE_CURVE('',#5874,#5874,#5328,.T.);
#7131=EDGE_CURVE('',#5874,#5875,#3146,.T.);
#7132=EDGE_CURVE('',#5875,#5875,#5329,.T.);
#7133=EDGE_CURVE('',#5876,#5876,#5330,.T.);
#7134=EDGE_CURVE('',#5876,#5877,#3147,.T.);
#7135=EDGE_CURVE('',#5877,#5877,#5331,.T.);
#7136=EDGE_CURVE('',#5878,#5878,#5332,.T.);
#7137=EDGE_CURVE('',#5878,#5879,#3148,.T.);
#7138=EDGE_CURVE('',#5879,#5879,#5333,.T.);
#7139=EDGE_CURVE('',#5880,#5880,#5334,.T.);
#7140=EDGE_CURVE('',#5880,#5881,#3149,.T.);
#7141=EDGE_CURVE('',#5881,#5881,#5335,.T.);
#7142=EDGE_CURVE('',#5882,#5882,#5336,.T.);
#7143=EDGE_CURVE('',#5882,#5883,#3150,.T.);
#7144=EDGE_CURVE('',#5883,#5883,#5337,.T.);
#7145=EDGE_CURVE('',#5884,#5884,#5338,.T.);
#7146=EDGE_CURVE('',#5884,#5885,#3151,.T.);
#7147=EDGE_CURVE('',#5885,#5885,#5339,.T.);
#7148=EDGE_CURVE('',#5886,#5886,#5340,.T.);
#7149=EDGE_CURVE('',#5886,#5887,#3152,.T.);
#7150=EDGE_CURVE('',#5887,#5887,#5341,.T.);
#7151=EDGE_CURVE('',#5888,#5888,#5342,.T.);
#7152=EDGE_CURVE('',#5888,#5889,#3153,.T.);
#7153=EDGE_CURVE('',#5889,#5889,#5343,.T.);
#7154=EDGE_CURVE('',#5890,#5890,#5344,.T.);
#7155=EDGE_CURVE('',#5891,#5891,#5345,.T.);
#7156=EDGE_CURVE('',#5891,#5890,#3154,.T.);
#7157=EDGE_CURVE('',#5892,#5892,#5346,.T.);
#7158=EDGE_CURVE('',#5892,#5893,#3155,.T.);
#7159=EDGE_CURVE('',#5893,#5893,#5347,.T.);
#7160=EDGE_CURVE('',#5894,#5894,#5348,.T.);
#7161=EDGE_CURVE('',#5894,#5895,#3156,.T.);
#7162=EDGE_CURVE('',#5895,#5895,#5349,.T.);
#7163=EDGE_CURVE('',#5896,#5896,#5350,.T.);
#7164=EDGE_CURVE('',#5896,#5897,#3157,.T.);
#7165=EDGE_CURVE('',#5897,#5897,#5351,.T.);
#7166=EDGE_CURVE('',#5898,#5898,#5352,.T.);
#7167=EDGE_CURVE('',#5898,#5899,#3158,.T.);
#7168=EDGE_CURVE('',#5899,#5899,#5353,.T.);
#7169=EDGE_CURVE('',#5900,#5900,#5354,.T.);
#7170=EDGE_CURVE('',#5900,#5901,#3159,.T.);
#7171=EDGE_CURVE('',#5901,#5901,#5355,.T.);
#7172=EDGE_CURVE('',#5902,#5902,#5356,.T.);
#7173=EDGE_CURVE('',#5902,#5903,#3160,.T.);
#7174=EDGE_CURVE('',#5903,#5903,#5357,.T.);
#7175=EDGE_CURVE('',#5904,#5904,#5358,.T.);
#7176=EDGE_CURVE('',#5904,#5905,#3161,.T.);
#7177=EDGE_CURVE('',#5905,#5905,#5359,.T.);
#7178=EDGE_CURVE('',#5906,#5906,#5360,.T.);
#7179=EDGE_CURVE('',#5906,#5907,#3162,.T.);
#7180=EDGE_CURVE('',#5907,#5907,#5361,.T.);
#7181=EDGE_CURVE('',#5908,#5909,#3163,.T.);
#7182=EDGE_CURVE('',#5910,#5908,#3164,.T.);
#7183=EDGE_CURVE('',#5910,#5911,#3165,.T.);
#7184=EDGE_CURVE('',#5909,#5911,#3166,.T.);
#7185=EDGE_CURVE('',#5912,#5913,#3167,.T.);
#7186=EDGE_CURVE('',#5914,#5912,#3168,.T.);
#7187=EDGE_CURVE('',#5915,#5914,#3169,.T.);
#7188=EDGE_CURVE('',#5913,#5915,#3170,.T.);
#7189=EDGE_CURVE('',#5915,#5916,#3171,.T.);
#7190=EDGE_CURVE('',#5917,#5914,#3172,.T.);
#7191=EDGE_CURVE('',#5916,#5917,#3173,.T.);
#7192=EDGE_CURVE('',#5918,#5910,#3174,.T.);
#7193=EDGE_CURVE('',#5918,#5919,#3175,.T.);
#7194=EDGE_CURVE('',#5911,#5919,#3176,.T.);
#7195=EDGE_CURVE('',#5908,#5920,#3177,.T.);
#7196=EDGE_CURVE('',#5921,#5920,#3178,.T.);
#7197=EDGE_CURVE('',#5913,#5921,#3179,.T.);
#7198=EDGE_CURVE('',#5916,#5918,#3180,.T.);
#7199=EDGE_CURVE('',#5909,#5922,#3181,.T.);
#7200=EDGE_CURVE('',#5920,#5922,#3182,.T.);
#7201=EDGE_CURVE('',#5912,#5923,#3183,.T.);
#7202=EDGE_CURVE('',#5922,#5923,#3184,.T.);
#7203=EDGE_CURVE('',#5919,#5917,#3185,.T.);
#7204=EDGE_CURVE('',#5923,#5921,#3186,.T.);
#7205=EDGE_CURVE('',#5924,#5924,#5362,.T.);
#7206=EDGE_CURVE('',#5924,#5925,#3187,.T.);
#7207=EDGE_CURVE('',#5925,#5925,#5363,.T.);
#7208=EDGE_CURVE('',#5926,#5926,#5364,.T.);
#7209=EDGE_CURVE('',#5926,#5927,#3188,.T.);
#7210=EDGE_CURVE('',#5927,#5927,#5365,.T.);
#7211=EDGE_CURVE('',#5928,#5928,#5366,.T.);
#7212=EDGE_CURVE('',#5928,#5929,#3189,.T.);
#7213=EDGE_CURVE('',#5929,#5929,#5367,.T.);
#7214=EDGE_CURVE('',#5930,#5930,#5368,.T.);
#7215=EDGE_CURVE('',#5930,#5931,#3190,.T.);
#7216=EDGE_CURVE('',#5931,#5931,#5369,.T.);
#7217=EDGE_CURVE('',#5932,#5932,#5370,.T.);
#7218=EDGE_CURVE('',#5932,#5933,#3191,.T.);
#7219=EDGE_CURVE('',#5933,#5933,#5371,.T.);
#7220=EDGE_CURVE('',#5934,#5934,#5372,.T.);
#7221=EDGE_CURVE('',#5934,#5935,#3192,.T.);
#7222=EDGE_CURVE('',#5935,#5935,#5373,.T.);
#7223=EDGE_CURVE('',#5936,#5936,#5374,.T.);
#7224=EDGE_CURVE('',#5936,#5937,#3193,.T.);
#7225=EDGE_CURVE('',#5937,#5937,#5375,.T.);
#7226=EDGE_CURVE('',#5938,#5938,#5376,.T.);
#7227=EDGE_CURVE('',#5938,#5939,#3194,.T.);
#7228=EDGE_CURVE('',#5939,#5939,#5377,.T.);
#7229=EDGE_CURVE('',#5940,#5940,#5378,.T.);
#7230=EDGE_CURVE('',#5940,#5941,#3195,.T.);
#7231=EDGE_CURVE('',#5941,#5941,#5379,.T.);
#7232=EDGE_CURVE('',#5942,#5942,#5380,.T.);
#7233=EDGE_CURVE('',#5942,#5943,#3196,.T.);
#7234=EDGE_CURVE('',#5943,#5943,#5381,.T.);
#7235=EDGE_CURVE('',#5944,#5944,#5382,.T.);
#7236=EDGE_CURVE('',#5944,#5945,#3197,.T.);
#7237=EDGE_CURVE('',#5945,#5945,#5383,.T.);
#7238=EDGE_CURVE('',#5946,#5946,#5384,.T.);
#7239=EDGE_CURVE('',#5946,#5947,#3198,.T.);
#7240=EDGE_CURVE('',#5947,#5947,#5385,.T.);
#7241=EDGE_CURVE('',#5948,#5948,#5386,.T.);
#7242=EDGE_CURVE('',#5949,#5949,#5387,.T.);
#7243=EDGE_CURVE('',#5949,#5948,#3199,.T.);
#7244=EDGE_CURVE('',#5950,#5950,#5388,.T.);
#7245=EDGE_CURVE('',#5950,#5951,#3200,.T.);
#7246=EDGE_CURVE('',#5951,#5951,#5389,.T.);
#7247=EDGE_CURVE('',#5952,#5952,#5390,.T.);
#7248=EDGE_CURVE('',#5953,#5953,#5391,.T.);
#7249=EDGE_CURVE('',#5953,#5954,#3201,.T.);
#7250=EDGE_CURVE('',#5954,#5954,#5392,.T.);
#7251=EDGE_CURVE('',#5952,#5953,#3202,.T.);
#7252=EDGE_CURVE('',#5955,#5956,#5393,.T.);
#7253=EDGE_CURVE('',#5956,#5955,#5394,.T.);
#7254=EDGE_CURVE('',#5956,#5957,#5395,.T.);
#7255=EDGE_CURVE('',#5958,#5957,#5396,.T.);
#7256=EDGE_CURVE('',#5957,#5958,#5397,.T.);
#7257=EDGE_CURVE('',#5958,#5959,#3203,.T.);
#7258=EDGE_CURVE('',#5959,#5959,#5398,.T.);
#7259=EDGE_CURVE('',#5960,#5960,#5399,.T.);
#7260=EDGE_CURVE('',#5960,#5961,#3204,.T.);
#7261=EDGE_CURVE('',#5961,#5961,#5400,.T.);
#7262=EDGE_CURVE('',#5961,#5962,#3205,.T.);
#7263=EDGE_CURVE('',#5962,#5962,#5401,.T.);
#7264=EDGE_CURVE('',#5963,#5963,#5402,.T.);
#7265=EDGE_CURVE('',#5963,#5955,#3206,.T.);
#7266=EDGE_CURVE('',#5964,#5964,#5403,.T.);
#7267=EDGE_CURVE('',#5964,#5960,#3207,.T.);
#7268=EDGE_CURVE('',#5965,#5966,#5404,.T.);
#7269=EDGE_CURVE('',#5966,#5965,#5405,.T.);
#7270=EDGE_CURVE('',#5966,#5967,#5406,.T.);
#7271=EDGE_CURVE('',#5968,#5967,#5407,.T.);
#7272=EDGE_CURVE('',#5967,#5968,#5408,.T.);
#7273=EDGE_CURVE('',#5969,#5969,#5409,.T.);
#7274=EDGE_CURVE('',#5969,#5968,#3208,.T.);
#7275=EDGE_CURVE('',#5970,#5970,#5410,.T.);
#7276=EDGE_CURVE('',#5971,#5971,#5411,.T.);
#7277=EDGE_CURVE('',#5972,#5972,#5412,.T.);
#7278=EDGE_CURVE('',#5972,#5970,#3209,.T.);
#7279=EDGE_CURVE('',#5973,#5973,#5413,.T.);
#7280=EDGE_CURVE('',#5973,#5972,#3210,.T.);
#7281=EDGE_CURVE('',#5974,#5974,#5414,.T.);
#7282=EDGE_CURVE('',#5974,#5973,#3211,.T.);
#7283=EDGE_CURVE('',#5965,#5971,#3212,.T.);
#7284=EDGE_CURVE('',#5975,#5976,#5415,.T.);
#7285=EDGE_CURVE('',#5977,#5978,#5416,.T.);
#7286=EDGE_CURVE('',#5979,#5980,#5417,.T.);
#7287=EDGE_CURVE('',#5981,#5982,#5418,.T.);
#7288=EDGE_CURVE('',#5983,#5984,#5419,.T.);
#7289=EDGE_CURVE('',#5985,#5986,#5420,.T.);
#7290=EDGE_CURVE('',#5987,#5988,#5421,.T.);
#7291=EDGE_CURVE('',#5989,#5990,#506,.T.);
#7292=EDGE_CURVE('',#5991,#5989,#5422,.T.);
#7293=EDGE_CURVE('',#5992,#5991,#507,.T.);
#7294=EDGE_CURVE('',#5990,#5992,#5423,.T.);
#7295=EDGE_CURVE('',#5993,#5991,#5424,.T.);
#7296=EDGE_CURVE('',#5993,#5994,#508,.T.);
#7297=EDGE_CURVE('',#5995,#5994,#5425,.T.);
#7298=EDGE_CURVE('',#5995,#5996,#509,.T.);
#7299=EDGE_CURVE('',#5997,#5996,#5426,.T.);
#7300=EDGE_CURVE('',#5997,#5998,#3213,.T.);
#7301=EDGE_CURVE('',#5998,#5998,#5427,.T.);
#7302=EDGE_CURVE('',#5999,#5997,#5428,.T.);
#7303=EDGE_CURVE('',#5999,#6000,#510,.T.);
#7304=EDGE_CURVE('',#6001,#6000,#5429,.T.);
#7305=EDGE_CURVE('',#6001,#6002,#511,.T.);
#7306=EDGE_CURVE('',#6003,#6002,#5430,.T.);
#7307=EDGE_CURVE('',#6003,#6004,#512,.T.);
#7308=EDGE_CURVE('',#6005,#6004,#5431,.T.);
#7309=EDGE_CURVE('',#6005,#6006,#513,.T.);
#7310=EDGE_CURVE('',#5992,#6006,#5432,.T.);
#7311=EDGE_CURVE('',#5989,#6007,#5433,.T.);
#7312=EDGE_CURVE('',#6007,#5993,#5434,.T.);
#7313=EDGE_CURVE('',#6008,#6007,#514,.T.);
#7314=EDGE_CURVE('',#5994,#6008,#5435,.T.);
#7315=EDGE_CURVE('',#6008,#6009,#5436,.T.);
#7316=EDGE_CURVE('',#6009,#5995,#5437,.T.);
#7317=EDGE_CURVE('',#6010,#6009,#515,.T.);
#7318=EDGE_CURVE('',#5996,#6010,#5438,.T.);
#7319=EDGE_CURVE('',#6010,#6011,#5439,.T.);
#7320=EDGE_CURVE('',#6011,#6012,#5440,.T.);
#7321=EDGE_CURVE('',#6012,#5999,#5441,.T.);
#7322=EDGE_CURVE('',#6013,#6012,#516,.T.);
#7323=EDGE_CURVE('',#6000,#6013,#5442,.T.);
#7324=EDGE_CURVE('',#6013,#6014,#5443,.T.);
#7325=EDGE_CURVE('',#6014,#6001,#5444,.T.);
#7326=EDGE_CURVE('',#6015,#6014,#517,.T.);
#7327=EDGE_CURVE('',#6002,#6015,#5445,.T.);
#7328=EDGE_CURVE('',#6015,#6016,#5446,.T.);
#7329=EDGE_CURVE('',#6016,#6003,#5447,.T.);
#7330=EDGE_CURVE('',#6017,#6016,#518,.T.);
#7331=EDGE_CURVE('',#6004,#6017,#5448,.T.);
#7332=EDGE_CURVE('',#6018,#6018,#5449,.T.);
#7333=EDGE_CURVE('',#6018,#6011,#3214,.T.);
#7334=EDGE_CURVE('',#6019,#5990,#5450,.T.);
#7335=EDGE_CURVE('',#6019,#6020,#519,.T.);
#7336=EDGE_CURVE('',#6017,#6020,#5451,.T.);
#7337=EDGE_CURVE('',#6006,#6019,#5452,.T.);
#7338=EDGE_CURVE('',#6020,#6005,#5453,.T.);
#7339=EDGE_CURVE('',#6021,#6021,#5454,.T.);
#7340=EDGE_CURVE('',#6022,#6022,#5455,.T.);
#7341=EDGE_CURVE('',#6023,#6023,#5456,.T.);
#7342=EDGE_CURVE('',#6023,#6021,#3215,.T.);
#7343=EDGE_CURVE('',#6024,#6024,#5457,.T.);
#7344=EDGE_CURVE('',#6024,#6022,#3216,.T.);
#7345=EDGE_CURVE('',#6025,#6025,#5458,.T.);
#7346=EDGE_CURVE('',#6026,#6026,#5459,.T.);
#7347=EDGE_CURVE('',#6027,#6027,#5460,.T.);
#7348=EDGE_CURVE('',#6027,#6025,#3217,.T.);
#7349=EDGE_CURVE('',#6028,#6028,#5461,.T.);
#7350=EDGE_CURVE('',#6028,#6026,#3218,.T.);
#7351=EDGE_CURVE('',#6029,#6030,#3219,.T.);
#7352=EDGE_CURVE('',#6030,#6031,#3220,.T.);
#7353=EDGE_CURVE('',#6031,#6032,#3221,.T.);
#7354=EDGE_CURVE('',#6029,#6032,#3222,.T.);
#7355=EDGE_CURVE('',#6030,#6033,#3223,.T.);
#7356=EDGE_CURVE('',#6033,#6034,#3224,.T.);
#7357=EDGE_CURVE('',#6034,#6031,#3225,.T.);
#7358=EDGE_CURVE('',#6033,#6035,#3226,.T.);
#7359=EDGE_CURVE('',#6035,#6036,#3227,.T.);
#7360=EDGE_CURVE('',#6036,#6034,#3228,.T.);
#7361=EDGE_CURVE('',#6035,#6037,#3229,.T.);
#7362=EDGE_CURVE('',#6037,#6038,#3230,.T.);
#7363=EDGE_CURVE('',#6038,#6036,#3231,.T.);
#7364=EDGE_CURVE('',#6037,#6039,#3232,.T.);
#7365=EDGE_CURVE('',#6039,#6040,#3233,.T.);
#7366=EDGE_CURVE('',#6040,#6038,#3234,.T.);
#7367=EDGE_CURVE('',#6039,#6029,#3235,.T.);
#7368=EDGE_CURVE('',#6032,#6040,#3236,.T.);
#7369=EDGE_CURVE('',#6041,#6041,#5462,.T.);
#7370=EDGE_CURVE('',#6042,#6042,#5463,.T.);
#7371=EDGE_CURVE('',#6043,#6043,#5464,.T.);
#7372=EDGE_CURVE('',#6043,#6042,#3237,.T.);
#7373=EDGE_CURVE('',#6044,#6044,#5465,.T.);
#7374=EDGE_CURVE('',#6044,#6043,#3238,.T.);
#7375=EDGE_CURVE('',#6045,#6045,#5466,.T.);
#7376=EDGE_CURVE('',#6045,#6044,#3239,.T.);
#7377=EDGE_CURVE('',#6046,#6046,#5467,.T.);
#7378=EDGE_CURVE('',#6047,#6047,#5468,.F.);
#7379=EDGE_CURVE('',#6047,#6046,#3240,.T.);
#7380=EDGE_CURVE('',#6041,#6047,#3241,.T.);
#7381=EDGE_CURVE('',#6048,#6048,#5469,.T.);
#7382=EDGE_CURVE('',#6048,#6049,#3242,.T.);
#7383=EDGE_CURVE('',#6049,#6049,#5470,.T.);
#7384=EDGE_CURVE('',#6050,#6051,#3243,.T.);
#7385=EDGE_CURVE('',#6052,#6050,#3244,.T.);
#7386=EDGE_CURVE('',#6053,#6052,#3245,.T.);
#7387=EDGE_CURVE('',#6053,#6051,#3246,.T.);
#7388=EDGE_CURVE('',#6054,#6055,#3247,.T.);
#7389=EDGE_CURVE('',#6054,#6056,#3248,.T.);
#7390=EDGE_CURVE('',#6057,#6056,#3249,.T.);
#7391=EDGE_CURVE('',#6055,#6057,#3250,.T.);
#7392=EDGE_CURVE('',#6051,#6058,#5471,.T.);
#7393=EDGE_CURVE('',#6059,#6053,#3251,.T.);
#7394=EDGE_CURVE('',#6059,#6060,#3252,.T.);
#7395=EDGE_CURVE('',#6056,#6060,#3253,.T.);
#7396=EDGE_CURVE('',#6058,#6054,#5472,.T.);
#7397=EDGE_CURVE('',#6055,#6061,#5473,.T.);
#7398=EDGE_CURVE('',#6062,#6057,#3254,.T.);
#7399=EDGE_CURVE('',#6063,#6062,#3255,.T.);
#7400=EDGE_CURVE('',#6052,#6063,#3256,.T.);
#7401=EDGE_CURVE('',#6061,#6050,#5474,.T.);
#7402=EDGE_CURVE('',#6063,#6064,#3257,.T.);
#7403=EDGE_CURVE('',#6065,#6062,#3258,.T.);
#7404=EDGE_CURVE('',#6064,#6065,#3259,.T.);
#7405=EDGE_CURVE('',#6064,#6066,#3260,.T.);
#7406=EDGE_CURVE('',#6067,#6065,#3261,.T.);
#7407=EDGE_CURVE('',#6066,#6067,#3262,.T.);
#7408=EDGE_CURVE('',#6066,#6068,#3263,.T.);
#7409=EDGE_CURVE('',#6069,#6067,#3264,.T.);
#7410=EDGE_CURVE('',#6068,#6069,#3265,.T.);
#7411=EDGE_CURVE('',#6068,#6070,#3266,.T.);
#7412=EDGE_CURVE('',#6071,#6069,#3267,.T.);
#7413=EDGE_CURVE('',#6070,#6071,#3268,.T.);
#7414=EDGE_CURVE('',#6070,#6072,#3269,.T.);
#7415=EDGE_CURVE('',#6073,#6071,#3270,.T.);
#7416=EDGE_CURVE('',#6072,#6073,#3271,.T.);
#7417=EDGE_CURVE('',#6072,#6074,#3272,.T.);
#7418=EDGE_CURVE('',#6075,#6073,#3273,.T.);
#7419=EDGE_CURVE('',#6074,#6075,#3274,.T.);
#7420=EDGE_CURVE('',#6074,#6076,#3275,.T.);
#7421=EDGE_CURVE('',#6077,#6075,#3276,.T.);
#7422=EDGE_CURVE('',#6076,#6077,#3277,.T.);
#7423=EDGE_CURVE('',#6076,#6078,#3278,.T.);
#7424=EDGE_CURVE('',#6079,#6077,#3279,.T.);
#7425=EDGE_CURVE('',#6078,#6079,#3280,.T.);
#7426=EDGE_CURVE('',#6078,#6080,#3281,.T.);
#7427=EDGE_CURVE('',#6081,#6079,#3282,.T.);
#7428=EDGE_CURVE('',#6080,#6081,#3283,.T.);
#7429=EDGE_CURVE('',#6080,#6082,#3284,.T.);
#7430=EDGE_CURVE('',#6083,#6081,#3285,.T.);
#7431=EDGE_CURVE('',#6082,#6083,#3286,.T.);
#7432=EDGE_CURVE('',#6082,#6084,#3287,.T.);
#7433=EDGE_CURVE('',#6085,#6083,#3288,.T.);
#7434=EDGE_CURVE('',#6084,#6085,#3289,.T.);
#7435=EDGE_CURVE('',#6084,#6086,#3290,.T.);
#7436=EDGE_CURVE('',#6087,#6085,#3291,.T.);
#7437=EDGE_CURVE('',#6086,#6087,#3292,.T.);
#7438=EDGE_CURVE('',#6086,#6088,#3293,.T.);
#7439=EDGE_CURVE('',#6089,#6087,#3294,.T.);
#7440=EDGE_CURVE('',#6088,#6089,#3295,.T.);
#7441=EDGE_CURVE('',#6088,#6090,#3296,.T.);
#7442=EDGE_CURVE('',#6091,#6089,#3297,.T.);
#7443=EDGE_CURVE('',#6090,#6091,#3298,.T.);
#7444=EDGE_CURVE('',#6090,#6092,#3299,.T.);
#7445=EDGE_CURVE('',#6093,#6091,#3300,.T.);
#7446=EDGE_CURVE('',#6092,#6093,#3301,.T.);
#7447=EDGE_CURVE('',#6092,#6094,#3302,.T.);
#7448=EDGE_CURVE('',#6095,#6093,#3303,.T.);
#7449=EDGE_CURVE('',#6094,#6095,#3304,.T.);
#7450=EDGE_CURVE('',#6094,#6096,#3305,.T.);
#7451=EDGE_CURVE('',#6097,#6095,#3306,.T.);
#7452=EDGE_CURVE('',#6096,#6097,#3307,.T.);
#7453=EDGE_CURVE('',#6096,#6098,#3308,.T.);
#7454=EDGE_CURVE('',#6099,#6097,#3309,.T.);
#7455=EDGE_CURVE('',#6098,#6099,#3310,.T.);
#7456=EDGE_CURVE('',#6098,#6100,#3311,.T.);
#7457=EDGE_CURVE('',#6101,#6099,#3312,.T.);
#7458=EDGE_CURVE('',#6100,#6101,#3313,.T.);
#7459=EDGE_CURVE('',#6100,#6102,#3314,.T.);
#7460=EDGE_CURVE('',#6103,#6101,#3315,.T.);
#7461=EDGE_CURVE('',#6102,#6103,#3316,.T.);
#7462=EDGE_CURVE('',#6102,#6104,#3317,.T.);
#7463=EDGE_CURVE('',#6105,#6103,#3318,.T.);
#7464=EDGE_CURVE('',#6104,#6105,#3319,.T.);
#7465=EDGE_CURVE('',#6104,#6106,#3320,.T.);
#7466=EDGE_CURVE('',#6107,#6105,#3321,.T.);
#7467=EDGE_CURVE('',#6106,#6107,#3322,.T.);
#7468=EDGE_CURVE('',#6106,#6108,#3323,.T.);
#7469=EDGE_CURVE('',#6109,#6107,#3324,.T.);
#7470=EDGE_CURVE('',#6108,#6109,#3325,.T.);
#7471=EDGE_CURVE('',#6108,#6110,#3326,.T.);
#7472=EDGE_CURVE('',#6111,#6109,#3327,.T.);
#7473=EDGE_CURVE('',#6110,#6111,#3328,.T.);
#7474=EDGE_CURVE('',#6110,#6112,#3329,.T.);
#7475=EDGE_CURVE('',#6113,#6111,#3330,.T.);
#7476=EDGE_CURVE('',#6112,#6113,#3331,.T.);
#7477=EDGE_CURVE('',#6112,#6114,#3332,.T.);
#7478=EDGE_CURVE('',#6115,#6113,#3333,.T.);
#7479=EDGE_CURVE('',#6114,#6115,#3334,.T.);
#7480=EDGE_CURVE('',#6114,#6116,#3335,.T.);
#7481=EDGE_CURVE('',#6117,#6115,#3336,.T.);
#7482=EDGE_CURVE('',#6116,#6117,#3337,.T.);
#7483=EDGE_CURVE('',#6116,#6118,#3338,.T.);
#7484=EDGE_CURVE('',#6119,#6117,#3339,.T.);
#7485=EDGE_CURVE('',#6118,#6119,#3340,.T.);
#7486=EDGE_CURVE('',#6118,#6120,#3341,.T.);
#7487=EDGE_CURVE('',#6121,#6119,#3342,.T.);
#7488=EDGE_CURVE('',#6120,#6121,#3343,.T.);
#7489=EDGE_CURVE('',#6120,#6122,#3344,.T.);
#7490=EDGE_CURVE('',#6123,#6121,#3345,.T.);
#7491=EDGE_CURVE('',#6122,#6123,#3346,.T.);
#7492=EDGE_CURVE('',#6122,#6124,#3347,.T.);
#7493=EDGE_CURVE('',#6125,#6123,#3348,.T.);
#7494=EDGE_CURVE('',#6124,#6125,#3349,.T.);
#7495=EDGE_CURVE('',#6124,#6126,#3350,.T.);
#7496=EDGE_CURVE('',#6127,#6125,#3351,.T.);
#7497=EDGE_CURVE('',#6126,#6127,#3352,.T.);
#7498=EDGE_CURVE('',#6126,#6128,#3353,.T.);
#7499=EDGE_CURVE('',#6129,#6127,#3354,.T.);
#7500=EDGE_CURVE('',#6128,#6129,#3355,.T.);
#7501=EDGE_CURVE('',#6128,#6130,#3356,.T.);
#7502=EDGE_CURVE('',#6131,#6129,#3357,.T.);
#7503=EDGE_CURVE('',#6130,#6131,#3358,.T.);
#7504=EDGE_CURVE('',#6130,#6132,#3359,.T.);
#7505=EDGE_CURVE('',#6133,#6131,#3360,.T.);
#7506=EDGE_CURVE('',#6132,#6133,#3361,.T.);
#7507=EDGE_CURVE('',#6132,#6134,#3362,.T.);
#7508=EDGE_CURVE('',#6135,#6133,#3363,.T.);
#7509=EDGE_CURVE('',#6134,#6135,#3364,.T.);
#7510=EDGE_CURVE('',#6134,#6136,#3365,.T.);
#7511=EDGE_CURVE('',#6137,#6135,#3366,.T.);
#7512=EDGE_CURVE('',#6136,#6137,#3367,.T.);
#7513=EDGE_CURVE('',#6136,#6138,#3368,.T.);
#7514=EDGE_CURVE('',#6139,#6137,#3369,.T.);
#7515=EDGE_CURVE('',#6138,#6139,#3370,.T.);
#7516=EDGE_CURVE('',#6138,#6140,#3371,.T.);
#7517=EDGE_CURVE('',#6141,#6139,#3372,.T.);
#7518=EDGE_CURVE('',#6140,#6141,#3373,.T.);
#7519=EDGE_CURVE('',#6140,#6142,#3374,.T.);
#7520=EDGE_CURVE('',#6143,#6141,#3375,.T.);
#7521=EDGE_CURVE('',#6142,#6143,#3376,.T.);
#7522=EDGE_CURVE('',#6142,#6144,#3377,.T.);
#7523=EDGE_CURVE('',#6145,#6143,#3378,.T.);
#7524=EDGE_CURVE('',#6144,#6145,#3379,.T.);
#7525=EDGE_CURVE('',#6144,#6146,#3380,.T.);
#7526=EDGE_CURVE('',#6147,#6145,#3381,.T.);
#7527=EDGE_CURVE('',#6146,#6147,#3382,.T.);
#7528=EDGE_CURVE('',#6146,#6148,#3383,.T.);
#7529=EDGE_CURVE('',#6149,#6147,#3384,.T.);
#7530=EDGE_CURVE('',#6148,#6149,#3385,.T.);
#7531=EDGE_CURVE('',#6148,#6150,#3386,.T.);
#7532=EDGE_CURVE('',#6151,#6149,#3387,.T.);
#7533=EDGE_CURVE('',#6150,#6151,#3388,.T.);
#7534=EDGE_CURVE('',#6150,#6152,#3389,.T.);
#7535=EDGE_CURVE('',#6153,#6151,#3390,.T.);
#7536=EDGE_CURVE('',#6152,#6153,#3391,.T.);
#7537=EDGE_CURVE('',#6152,#6154,#3392,.T.);
#7538=EDGE_CURVE('',#6155,#6153,#3393,.T.);
#7539=EDGE_CURVE('',#6154,#6155,#3394,.T.);
#7540=EDGE_CURVE('',#6154,#6156,#3395,.T.);
#7541=EDGE_CURVE('',#6157,#6155,#3396,.T.);
#7542=EDGE_CURVE('',#6156,#6157,#3397,.T.);
#7543=EDGE_CURVE('',#6156,#6158,#3398,.T.);
#7544=EDGE_CURVE('',#6159,#6157,#3399,.T.);
#7545=EDGE_CURVE('',#6158,#6159,#3400,.T.);
#7546=EDGE_CURVE('',#6158,#6160,#3401,.T.);
#7547=EDGE_CURVE('',#6161,#6159,#3402,.T.);
#7548=EDGE_CURVE('',#6160,#6161,#3403,.T.);
#7549=EDGE_CURVE('',#6160,#6162,#3404,.T.);
#7550=EDGE_CURVE('',#6163,#6161,#3405,.T.);
#7551=EDGE_CURVE('',#6162,#6163,#3406,.T.);
#7552=EDGE_CURVE('',#6162,#6164,#3407,.T.);
#7553=EDGE_CURVE('',#6165,#6163,#3408,.T.);
#7554=EDGE_CURVE('',#6164,#6165,#3409,.T.);
#7555=EDGE_CURVE('',#6164,#6166,#3410,.T.);
#7556=EDGE_CURVE('',#6167,#6165,#3411,.T.);
#7557=EDGE_CURVE('',#6166,#6167,#3412,.T.);
#7558=EDGE_CURVE('',#6166,#6168,#3413,.T.);
#7559=EDGE_CURVE('',#6169,#6167,#3414,.T.);
#7560=EDGE_CURVE('',#6168,#6169,#3415,.T.);
#7561=EDGE_CURVE('',#6168,#6170,#3416,.T.);
#7562=EDGE_CURVE('',#6171,#6169,#3417,.T.);
#7563=EDGE_CURVE('',#6170,#6171,#3418,.T.);
#7564=EDGE_CURVE('',#6170,#6172,#3419,.T.);
#7565=EDGE_CURVE('',#6173,#6171,#3420,.T.);
#7566=EDGE_CURVE('',#6172,#6173,#3421,.T.);
#7567=EDGE_CURVE('',#6172,#6174,#3422,.T.);
#7568=EDGE_CURVE('',#6175,#6173,#3423,.T.);
#7569=EDGE_CURVE('',#6174,#6175,#3424,.T.);
#7570=EDGE_CURVE('',#6174,#6176,#3425,.T.);
#7571=EDGE_CURVE('',#6177,#6175,#3426,.T.);
#7572=EDGE_CURVE('',#6176,#6177,#3427,.T.);
#7573=EDGE_CURVE('',#6176,#6178,#3428,.T.);
#7574=EDGE_CURVE('',#6179,#6177,#3429,.T.);
#7575=EDGE_CURVE('',#6178,#6179,#3430,.T.);
#7576=EDGE_CURVE('',#6178,#6180,#3431,.T.);
#7577=EDGE_CURVE('',#6181,#6179,#3432,.T.);
#7578=EDGE_CURVE('',#6180,#6181,#3433,.T.);
#7579=EDGE_CURVE('',#6180,#6182,#3434,.T.);
#7580=EDGE_CURVE('',#6183,#6181,#3435,.T.);
#7581=EDGE_CURVE('',#6182,#6183,#3436,.T.);
#7582=EDGE_CURVE('',#6182,#6184,#3437,.T.);
#7583=EDGE_CURVE('',#6185,#6183,#3438,.T.);
#7584=EDGE_CURVE('',#6184,#6185,#3439,.T.);
#7585=EDGE_CURVE('',#6184,#6186,#3440,.T.);
#7586=EDGE_CURVE('',#6187,#6185,#3441,.T.);
#7587=EDGE_CURVE('',#6186,#6187,#3442,.T.);
#7588=EDGE_CURVE('',#6186,#6188,#3443,.T.);
#7589=EDGE_CURVE('',#6189,#6187,#3444,.T.);
#7590=EDGE_CURVE('',#6188,#6189,#3445,.T.);
#7591=EDGE_CURVE('',#6188,#6190,#3446,.T.);
#7592=EDGE_CURVE('',#6191,#6189,#3447,.T.);
#7593=EDGE_CURVE('',#6190,#6191,#3448,.T.);
#7594=EDGE_CURVE('',#6190,#6192,#3449,.T.);
#7595=EDGE_CURVE('',#6193,#6191,#3450,.T.);
#7596=EDGE_CURVE('',#6192,#6193,#3451,.T.);
#7597=EDGE_CURVE('',#6192,#6194,#3452,.T.);
#7598=EDGE_CURVE('',#6195,#6193,#3453,.T.);
#7599=EDGE_CURVE('',#6194,#6195,#3454,.T.);
#7600=EDGE_CURVE('',#6194,#6196,#3455,.T.);
#7601=EDGE_CURVE('',#6197,#6195,#3456,.T.);
#7602=EDGE_CURVE('',#6196,#6197,#3457,.T.);
#7603=EDGE_CURVE('',#6196,#6198,#3458,.T.);
#7604=EDGE_CURVE('',#6199,#6197,#3459,.T.);
#7605=EDGE_CURVE('',#6198,#6199,#3460,.T.);
#7606=EDGE_CURVE('',#6198,#6200,#3461,.T.);
#7607=EDGE_CURVE('',#6201,#6199,#3462,.T.);
#7608=EDGE_CURVE('',#6200,#6201,#3463,.T.);
#7609=EDGE_CURVE('',#6200,#6202,#3464,.T.);
#7610=EDGE_CURVE('',#6203,#6201,#3465,.T.);
#7611=EDGE_CURVE('',#6202,#6203,#3466,.T.);
#7612=EDGE_CURVE('',#6202,#6204,#3467,.T.);
#7613=EDGE_CURVE('',#6205,#6203,#3468,.T.);
#7614=EDGE_CURVE('',#6204,#6205,#3469,.T.);
#7615=EDGE_CURVE('',#6204,#6206,#3470,.T.);
#7616=EDGE_CURVE('',#6207,#6205,#3471,.T.);
#7617=EDGE_CURVE('',#6206,#6207,#3472,.T.);
#7618=EDGE_CURVE('',#6206,#6208,#3473,.T.);
#7619=EDGE_CURVE('',#6209,#6207,#3474,.T.);
#7620=EDGE_CURVE('',#6208,#6209,#3475,.T.);
#7621=EDGE_CURVE('',#6208,#6210,#3476,.T.);
#7622=EDGE_CURVE('',#6211,#6209,#3477,.T.);
#7623=EDGE_CURVE('',#6210,#6211,#3478,.T.);
#7624=EDGE_CURVE('',#6210,#6212,#3479,.T.);
#7625=EDGE_CURVE('',#6213,#6211,#3480,.T.);
#7626=EDGE_CURVE('',#6212,#6213,#3481,.T.);
#7627=EDGE_CURVE('',#6212,#6214,#3482,.T.);
#7628=EDGE_CURVE('',#6215,#6213,#3483,.T.);
#7629=EDGE_CURVE('',#6214,#6215,#3484,.T.);
#7630=EDGE_CURVE('',#6214,#6216,#3485,.T.);
#7631=EDGE_CURVE('',#6217,#6215,#3486,.T.);
#7632=EDGE_CURVE('',#6216,#6217,#3487,.T.);
#7633=EDGE_CURVE('',#6216,#6218,#3488,.T.);
#7634=EDGE_CURVE('',#6219,#6217,#3489,.T.);
#7635=EDGE_CURVE('',#6218,#6219,#3490,.T.);
#7636=EDGE_CURVE('',#6218,#6220,#3491,.T.);
#7637=EDGE_CURVE('',#6221,#6219,#3492,.T.);
#7638=EDGE_CURVE('',#6220,#6221,#3493,.T.);
#7639=EDGE_CURVE('',#6220,#6222,#3494,.T.);
#7640=EDGE_CURVE('',#6223,#6221,#3495,.T.);
#7641=EDGE_CURVE('',#6222,#6223,#3496,.T.);
#7642=EDGE_CURVE('',#6222,#6224,#3497,.T.);
#7643=EDGE_CURVE('',#6225,#6223,#3498,.T.);
#7644=EDGE_CURVE('',#6224,#6225,#3499,.T.);
#7645=EDGE_CURVE('',#6224,#6226,#3500,.T.);
#7646=EDGE_CURVE('',#6227,#6225,#3501,.T.);
#7647=EDGE_CURVE('',#6226,#6227,#3502,.T.);
#7648=EDGE_CURVE('',#6226,#6228,#3503,.T.);
#7649=EDGE_CURVE('',#6229,#6227,#3504,.T.);
#7650=EDGE_CURVE('',#6228,#6229,#3505,.T.);
#7651=EDGE_CURVE('',#6228,#6230,#3506,.T.);
#7652=EDGE_CURVE('',#6231,#6229,#3507,.T.);
#7653=EDGE_CURVE('',#6230,#6231,#3508,.T.);
#7654=EDGE_CURVE('',#6230,#6232,#3509,.T.);
#7655=EDGE_CURVE('',#6233,#6231,#3510,.T.);
#7656=EDGE_CURVE('',#6232,#6233,#3511,.T.);
#7657=EDGE_CURVE('',#6232,#6234,#3512,.T.);
#7658=EDGE_CURVE('',#6235,#6233,#3513,.T.);
#7659=EDGE_CURVE('',#6234,#6235,#3514,.T.);
#7660=EDGE_CURVE('',#6234,#6236,#3515,.T.);
#7661=EDGE_CURVE('',#6237,#6235,#3516,.T.);
#7662=EDGE_CURVE('',#6236,#6237,#3517,.T.);
#7663=EDGE_CURVE('',#6236,#6238,#3518,.T.);
#7664=EDGE_CURVE('',#6239,#6237,#3519,.T.);
#7665=EDGE_CURVE('',#6238,#6239,#3520,.T.);
#7666=EDGE_CURVE('',#6238,#6240,#3521,.T.);
#7667=EDGE_CURVE('',#6241,#6239,#3522,.T.);
#7668=EDGE_CURVE('',#6240,#6241,#3523,.T.);
#7669=EDGE_CURVE('',#6240,#6242,#3524,.T.);
#7670=EDGE_CURVE('',#6243,#6241,#3525,.T.);
#7671=EDGE_CURVE('',#6242,#6243,#3526,.T.);
#7672=EDGE_CURVE('',#6242,#6244,#3527,.T.);
#7673=EDGE_CURVE('',#6245,#6243,#3528,.T.);
#7674=EDGE_CURVE('',#6244,#6245,#3529,.T.);
#7675=EDGE_CURVE('',#6244,#6246,#3530,.T.);
#7676=EDGE_CURVE('',#6247,#6245,#3531,.T.);
#7677=EDGE_CURVE('',#6246,#6247,#3532,.T.);
#7678=EDGE_CURVE('',#6246,#6248,#3533,.T.);
#7679=EDGE_CURVE('',#6249,#6247,#3534,.T.);
#7680=EDGE_CURVE('',#6248,#6249,#3535,.T.);
#7681=EDGE_CURVE('',#6248,#6250,#3536,.T.);
#7682=EDGE_CURVE('',#6251,#6249,#3537,.T.);
#7683=EDGE_CURVE('',#6250,#6251,#3538,.T.);
#7684=EDGE_CURVE('',#6250,#6252,#3539,.T.);
#7685=EDGE_CURVE('',#6253,#6251,#3540,.T.);
#7686=EDGE_CURVE('',#6252,#6253,#3541,.T.);
#7687=EDGE_CURVE('',#6252,#6254,#3542,.T.);
#7688=EDGE_CURVE('',#6255,#6253,#3543,.T.);
#7689=EDGE_CURVE('',#6254,#6255,#3544,.T.);
#7690=EDGE_CURVE('',#6254,#6256,#3545,.T.);
#7691=EDGE_CURVE('',#6257,#6255,#3546,.T.);
#7692=EDGE_CURVE('',#6256,#6257,#3547,.T.);
#7693=EDGE_CURVE('',#6256,#6258,#3548,.T.);
#7694=EDGE_CURVE('',#6259,#6257,#3549,.T.);
#7695=EDGE_CURVE('',#6258,#6259,#3550,.T.);
#7696=EDGE_CURVE('',#6258,#6260,#3551,.T.);
#7697=EDGE_CURVE('',#6261,#6259,#3552,.T.);
#7698=EDGE_CURVE('',#6260,#6261,#3553,.T.);
#7699=EDGE_CURVE('',#6260,#6262,#3554,.T.);
#7700=EDGE_CURVE('',#6263,#6261,#3555,.T.);
#7701=EDGE_CURVE('',#6262,#6263,#3556,.T.);
#7702=EDGE_CURVE('',#6262,#6264,#3557,.T.);
#7703=EDGE_CURVE('',#6265,#6263,#3558,.T.);
#7704=EDGE_CURVE('',#6264,#6265,#3559,.T.);
#7705=EDGE_CURVE('',#6264,#6266,#3560,.T.);
#7706=EDGE_CURVE('',#6267,#6265,#3561,.T.);
#7707=EDGE_CURVE('',#6266,#6267,#3562,.T.);
#7708=EDGE_CURVE('',#6266,#6268,#3563,.T.);
#7709=EDGE_CURVE('',#6269,#6267,#3564,.T.);
#7710=EDGE_CURVE('',#6268,#6269,#3565,.T.);
#7711=EDGE_CURVE('',#6268,#6270,#3566,.T.);
#7712=EDGE_CURVE('',#6271,#6269,#3567,.T.);
#7713=EDGE_CURVE('',#6270,#6271,#3568,.T.);
#7714=EDGE_CURVE('',#6270,#6272,#3569,.T.);
#7715=EDGE_CURVE('',#6273,#6271,#3570,.T.);
#7716=EDGE_CURVE('',#6272,#6273,#3571,.T.);
#7717=EDGE_CURVE('',#6272,#6274,#3572,.T.);
#7718=EDGE_CURVE('',#6275,#6273,#3573,.T.);
#7719=EDGE_CURVE('',#6274,#6275,#3574,.T.);
#7720=EDGE_CURVE('',#6274,#6276,#3575,.T.);
#7721=EDGE_CURVE('',#6277,#6275,#3576,.T.);
#7722=EDGE_CURVE('',#6276,#6277,#3577,.T.);
#7723=EDGE_CURVE('',#6276,#6278,#3578,.T.);
#7724=EDGE_CURVE('',#6279,#6277,#3579,.T.);
#7725=EDGE_CURVE('',#6278,#6279,#3580,.T.);
#7726=EDGE_CURVE('',#6278,#6280,#3581,.T.);
#7727=EDGE_CURVE('',#6281,#6279,#3582,.T.);
#7728=EDGE_CURVE('',#6280,#6281,#3583,.T.);
#7729=EDGE_CURVE('',#6280,#6282,#3584,.T.);
#7730=EDGE_CURVE('',#6283,#6281,#3585,.T.);
#7731=EDGE_CURVE('',#6282,#6283,#3586,.T.);
#7732=EDGE_CURVE('',#6282,#6284,#3587,.T.);
#7733=EDGE_CURVE('',#6285,#6283,#3588,.T.);
#7734=EDGE_CURVE('',#6284,#6285,#3589,.T.);
#7735=EDGE_CURVE('',#6284,#6286,#3590,.T.);
#7736=EDGE_CURVE('',#6287,#6285,#3591,.T.);
#7737=EDGE_CURVE('',#6286,#6287,#3592,.T.);
#7738=EDGE_CURVE('',#6286,#6288,#3593,.T.);
#7739=EDGE_CURVE('',#6289,#6287,#3594,.T.);
#7740=EDGE_CURVE('',#6288,#6289,#3595,.T.);
#7741=EDGE_CURVE('',#6288,#6290,#3596,.T.);
#7742=EDGE_CURVE('',#6291,#6289,#3597,.T.);
#7743=EDGE_CURVE('',#6290,#6291,#3598,.T.);
#7744=EDGE_CURVE('',#6290,#6292,#3599,.T.);
#7745=EDGE_CURVE('',#6293,#6291,#3600,.T.);
#7746=EDGE_CURVE('',#6292,#6293,#3601,.T.);
#7747=EDGE_CURVE('',#6292,#6294,#3602,.T.);
#7748=EDGE_CURVE('',#6295,#6293,#3603,.T.);
#7749=EDGE_CURVE('',#6294,#6295,#3604,.T.);
#7750=EDGE_CURVE('',#6294,#6296,#3605,.T.);
#7751=EDGE_CURVE('',#6297,#6295,#3606,.T.);
#7752=EDGE_CURVE('',#6296,#6297,#3607,.T.);
#7753=EDGE_CURVE('',#6296,#6298,#3608,.T.);
#7754=EDGE_CURVE('',#6299,#6297,#3609,.T.);
#7755=EDGE_CURVE('',#6298,#6299,#3610,.T.);
#7756=EDGE_CURVE('',#6298,#6300,#3611,.T.);
#7757=EDGE_CURVE('',#6301,#6299,#3612,.T.);
#7758=EDGE_CURVE('',#6300,#6301,#3613,.T.);
#7759=EDGE_CURVE('',#6300,#6302,#3614,.T.);
#7760=EDGE_CURVE('',#6303,#6301,#3615,.T.);
#7761=EDGE_CURVE('',#6302,#6303,#3616,.T.);
#7762=EDGE_CURVE('',#6302,#6304,#3617,.T.);
#7763=EDGE_CURVE('',#6305,#6303,#3618,.T.);
#7764=EDGE_CURVE('',#6304,#6305,#3619,.T.);
#7765=EDGE_CURVE('',#6304,#6306,#3620,.T.);
#7766=EDGE_CURVE('',#6307,#6305,#3621,.T.);
#7767=EDGE_CURVE('',#6306,#6307,#3622,.T.);
#7768=EDGE_CURVE('',#6306,#6308,#3623,.T.);
#7769=EDGE_CURVE('',#6309,#6307,#3624,.T.);
#7770=EDGE_CURVE('',#6308,#6309,#3625,.T.);
#7771=EDGE_CURVE('',#6308,#6310,#3626,.T.);
#7772=EDGE_CURVE('',#6311,#6309,#3627,.T.);
#7773=EDGE_CURVE('',#6310,#6311,#3628,.T.);
#7774=EDGE_CURVE('',#6310,#6312,#3629,.T.);
#7775=EDGE_CURVE('',#6313,#6311,#3630,.T.);
#7776=EDGE_CURVE('',#6312,#6313,#3631,.T.);
#7777=EDGE_CURVE('',#6312,#6314,#3632,.T.);
#7778=EDGE_CURVE('',#6315,#6313,#3633,.T.);
#7779=EDGE_CURVE('',#6314,#6315,#3634,.T.);
#7780=EDGE_CURVE('',#6314,#6316,#3635,.T.);
#7781=EDGE_CURVE('',#6317,#6315,#3636,.T.);
#7782=EDGE_CURVE('',#6316,#6317,#3637,.T.);
#7783=EDGE_CURVE('',#6316,#6318,#3638,.T.);
#7784=EDGE_CURVE('',#6319,#6317,#3639,.T.);
#7785=EDGE_CURVE('',#6318,#6319,#3640,.T.);
#7786=EDGE_CURVE('',#6318,#6320,#3641,.T.);
#7787=EDGE_CURVE('',#6321,#6319,#3642,.T.);
#7788=EDGE_CURVE('',#6320,#6321,#3643,.T.);
#7789=EDGE_CURVE('',#6320,#6322,#3644,.T.);
#7790=EDGE_CURVE('',#6323,#6321,#3645,.T.);
#7791=EDGE_CURVE('',#6322,#6323,#3646,.T.);
#7792=EDGE_CURVE('',#6322,#6324,#3647,.T.);
#7793=EDGE_CURVE('',#6325,#6323,#3648,.T.);
#7794=EDGE_CURVE('',#6324,#6325,#3649,.T.);
#7795=EDGE_CURVE('',#6324,#6326,#3650,.T.);
#7796=EDGE_CURVE('',#6327,#6325,#3651,.T.);
#7797=EDGE_CURVE('',#6326,#6327,#3652,.T.);
#7798=EDGE_CURVE('',#6326,#6328,#3653,.T.);
#7799=EDGE_CURVE('',#6329,#6327,#3654,.T.);
#7800=EDGE_CURVE('',#6328,#6329,#3655,.T.);
#7801=EDGE_CURVE('',#6328,#6330,#3656,.T.);
#7802=EDGE_CURVE('',#6331,#6329,#3657,.T.);
#7803=EDGE_CURVE('',#6330,#6331,#3658,.T.);
#7804=EDGE_CURVE('',#6330,#6332,#3659,.T.);
#7805=EDGE_CURVE('',#6333,#6331,#3660,.T.);
#7806=EDGE_CURVE('',#6332,#6333,#3661,.T.);
#7807=EDGE_CURVE('',#6332,#6334,#3662,.T.);
#7808=EDGE_CURVE('',#6335,#6333,#3663,.T.);
#7809=EDGE_CURVE('',#6334,#6335,#3664,.T.);
#7810=EDGE_CURVE('',#6334,#6336,#3665,.T.);
#7811=EDGE_CURVE('',#6337,#6335,#3666,.T.);
#7812=EDGE_CURVE('',#6336,#6337,#3667,.T.);
#7813=EDGE_CURVE('',#6336,#6338,#3668,.T.);
#7814=EDGE_CURVE('',#6339,#6337,#3669,.T.);
#7815=EDGE_CURVE('',#6338,#6339,#3670,.T.);
#7816=EDGE_CURVE('',#6338,#6340,#3671,.T.);
#7817=EDGE_CURVE('',#6341,#6339,#3672,.T.);
#7818=EDGE_CURVE('',#6340,#6341,#3673,.T.);
#7819=EDGE_CURVE('',#6340,#6342,#3674,.T.);
#7820=EDGE_CURVE('',#6343,#6341,#3675,.T.);
#7821=EDGE_CURVE('',#6342,#6343,#3676,.T.);
#7822=EDGE_CURVE('',#6342,#6344,#3677,.T.);
#7823=EDGE_CURVE('',#6345,#6343,#3678,.T.);
#7824=EDGE_CURVE('',#6344,#6345,#3679,.T.);
#7825=EDGE_CURVE('',#6344,#6346,#3680,.T.);
#7826=EDGE_CURVE('',#6347,#6345,#3681,.T.);
#7827=EDGE_CURVE('',#6346,#6347,#3682,.T.);
#7828=EDGE_CURVE('',#6346,#6348,#3683,.T.);
#7829=EDGE_CURVE('',#6349,#6347,#3684,.T.);
#7830=EDGE_CURVE('',#6348,#6349,#3685,.T.);
#7831=EDGE_CURVE('',#6348,#6350,#3686,.T.);
#7832=EDGE_CURVE('',#6351,#6349,#3687,.T.);
#7833=EDGE_CURVE('',#6350,#6351,#3688,.T.);
#7834=EDGE_CURVE('',#6350,#6352,#3689,.T.);
#7835=EDGE_CURVE('',#6353,#6351,#3690,.T.);
#7836=EDGE_CURVE('',#6352,#6353,#3691,.T.);
#7837=EDGE_CURVE('',#6352,#6354,#3692,.T.);
#7838=EDGE_CURVE('',#6355,#6353,#3693,.T.);
#7839=EDGE_CURVE('',#6354,#6355,#3694,.T.);
#7840=EDGE_CURVE('',#6354,#6356,#3695,.T.);
#7841=EDGE_CURVE('',#6357,#6355,#3696,.T.);
#7842=EDGE_CURVE('',#6356,#6357,#3697,.T.);
#7843=EDGE_CURVE('',#6356,#6358,#3698,.T.);
#7844=EDGE_CURVE('',#6359,#6357,#3699,.T.);
#7845=EDGE_CURVE('',#6358,#6359,#3700,.T.);
#7846=EDGE_CURVE('',#6358,#6360,#3701,.T.);
#7847=EDGE_CURVE('',#6361,#6359,#3702,.T.);
#7848=EDGE_CURVE('',#6360,#6361,#3703,.T.);
#7849=EDGE_CURVE('',#6360,#6362,#3704,.T.);
#7850=EDGE_CURVE('',#6363,#6361,#3705,.T.);
#7851=EDGE_CURVE('',#6362,#6363,#3706,.T.);
#7852=EDGE_CURVE('',#6362,#6364,#3707,.T.);
#7853=EDGE_CURVE('',#6365,#6363,#3708,.T.);
#7854=EDGE_CURVE('',#6364,#6365,#3709,.T.);
#7855=EDGE_CURVE('',#6364,#6366,#3710,.T.);
#7856=EDGE_CURVE('',#6367,#6365,#3711,.T.);
#7857=EDGE_CURVE('',#6366,#6367,#3712,.T.);
#7858=EDGE_CURVE('',#6366,#6368,#3713,.T.);
#7859=EDGE_CURVE('',#6369,#6367,#3714,.T.);
#7860=EDGE_CURVE('',#6368,#6369,#3715,.T.);
#7861=EDGE_CURVE('',#6368,#6370,#3716,.T.);
#7862=EDGE_CURVE('',#6371,#6369,#3717,.T.);
#7863=EDGE_CURVE('',#6370,#6371,#3718,.T.);
#7864=EDGE_CURVE('',#6370,#6372,#3719,.T.);
#7865=EDGE_CURVE('',#6373,#6371,#3720,.T.);
#7866=EDGE_CURVE('',#6372,#6373,#3721,.T.);
#7867=EDGE_CURVE('',#6372,#6374,#3722,.T.);
#7868=EDGE_CURVE('',#6375,#6373,#3723,.T.);
#7869=EDGE_CURVE('',#6374,#6375,#3724,.T.);
#7870=EDGE_CURVE('',#6374,#6376,#3725,.T.);
#7871=EDGE_CURVE('',#6377,#6375,#3726,.T.);
#7872=EDGE_CURVE('',#6376,#6377,#3727,.T.);
#7873=EDGE_CURVE('',#6376,#6378,#3728,.T.);
#7874=EDGE_CURVE('',#6379,#6377,#3729,.T.);
#7875=EDGE_CURVE('',#6378,#6379,#3730,.T.);
#7876=EDGE_CURVE('',#6378,#6380,#3731,.T.);
#7877=EDGE_CURVE('',#6381,#6379,#3732,.T.);
#7878=EDGE_CURVE('',#6380,#6381,#3733,.T.);
#7879=EDGE_CURVE('',#6380,#6382,#3734,.T.);
#7880=EDGE_CURVE('',#6383,#6381,#3735,.T.);
#7881=EDGE_CURVE('',#6382,#6383,#3736,.T.);
#7882=EDGE_CURVE('',#6382,#6059,#3737,.T.);
#7883=EDGE_CURVE('',#6060,#6383,#3738,.T.);
#7884=EDGE_CURVE('',#6384,#6384,#5475,.T.);
#7885=EDGE_CURVE('',#6384,#6061,#3739,.T.);
#7886=EDGE_CURVE('',#6058,#6385,#3740,.T.);
#7887=EDGE_CURVE('',#6385,#6385,#5476,.T.);
#7888=EDGE_CURVE('',#6386,#6387,#3741,.T.);
#7889=EDGE_CURVE('',#6386,#6387,#5477,.T.);
#7890=EDGE_CURVE('',#6388,#6386,#520,.T.);
#7891=EDGE_CURVE('',#6389,#6388,#5478,.T.);
#7892=EDGE_CURVE('',#6390,#6389,#521,.T.);
#7893=EDGE_CURVE('',#6390,#6391,#3742,.T.);
#7894=EDGE_CURVE('',#6392,#6391,#522,.T.);
#7895=EDGE_CURVE('',#6391,#6392,#523,.T.);
#7896=EDGE_CURVE('',#6387,#6390,#524,.T.);
#7897=EDGE_CURVE('',#6389,#6388,#3743,.T.);
#7898=EDGE_CURVE('',#6393,#6393,#5479,.T.);
#7899=EDGE_CURVE('',#6393,#6394,#3744,.T.);
#7900=EDGE_CURVE('',#6394,#6394,#5480,.T.);
#7901=EDGE_CURVE('',#6395,#6395,#5481,.T.);
#7902=EDGE_CURVE('',#6395,#6396,#3745,.T.);
#7903=EDGE_CURVE('',#6396,#6396,#5482,.T.);
#7904=EDGE_CURVE('',#6397,#6397,#5483,.T.);
#7905=EDGE_CURVE('',#6397,#6398,#3746,.T.);
#7906=EDGE_CURVE('',#6398,#6398,#5484,.T.);
#7907=EDGE_CURVE('',#6399,#6399,#5485,.T.);
#7908=EDGE_CURVE('',#6399,#6400,#3747,.T.);
#7909=EDGE_CURVE('',#6400,#6400,#5486,.T.);
#7910=EDGE_CURVE('',#6401,#6401,#5487,.T.);
#7911=EDGE_CURVE('',#6401,#6402,#3748,.T.);
#7912=EDGE_CURVE('',#6402,#6402,#5488,.T.);
#7913=EDGE_CURVE('',#6403,#6404,#525,.T.);
#7914=EDGE_CURVE('',#6404,#6403,#526,.T.);
#7915=EDGE_CURVE('',#6404,#6405,#3749,.T.);
#7916=EDGE_CURVE('',#6406,#6405,#527,.T.);
#7917=EDGE_CURVE('',#6405,#6406,#528,.T.);
#7918=EDGE_CURVE('',#6407,#6408,#3750,.T.);
#7919=EDGE_CURVE('',#6407,#6409,#3751,.T.);
#7920=EDGE_CURVE('',#6410,#6409,#3752,.T.);
#7921=EDGE_CURVE('',#6408,#6410,#3753,.T.);
#7922=EDGE_CURVE('',#6411,#6412,#3754,.T.);
#7923=EDGE_CURVE('',#6411,#6413,#3755,.T.);
#7924=EDGE_CURVE('',#6414,#6413,#3756,.T.);
#7925=EDGE_CURVE('',#6412,#6414,#3757,.T.);
#7926=EDGE_CURVE('',#6415,#6407,#3758,.T.);
#7927=EDGE_CURVE('',#6416,#6415,#3759,.T.);
#7928=EDGE_CURVE('',#6409,#6416,#3760,.T.);
#7929=EDGE_CURVE('',#6417,#6411,#3761,.T.);
#7930=EDGE_CURVE('',#6418,#6417,#3762,.T.);
#7931=EDGE_CURVE('',#6413,#6418,#3763,.T.);
#7932=EDGE_CURVE('',#6416,#6414,#5489,.T.);
#7933=EDGE_CURVE('',#6418,#6410,#5490,.T.);
#7934=EDGE_CURVE('',#6417,#6408,#5491,.T.);
#7935=EDGE_CURVE('',#6415,#6412,#5492,.T.);
#7936=EDGE_CURVE('',#6419,#6420,#3764,.T.);
#7937=EDGE_CURVE('',#6419,#6421,#3765,.T.);
#7938=EDGE_CURVE('',#6421,#6422,#3766,.T.);
#7939=EDGE_CURVE('',#6420,#6422,#3767,.T.);
#7940=EDGE_CURVE('',#6423,#6419,#3768,.T.);
#7941=EDGE_CURVE('',#6423,#6424,#3769,.T.);
#7942=EDGE_CURVE('',#6424,#6421,#3770,.T.);
#7943=EDGE_CURVE('',#6425,#6423,#3771,.T.);
#7944=EDGE_CURVE('',#6425,#6426,#3772,.T.);
#7945=EDGE_CURVE('',#6426,#6424,#3773,.T.);
#7946=EDGE_CURVE('',#6427,#6425,#3774,.T.);
#7947=EDGE_CURVE('',#6427,#6428,#3775,.T.);
#7948=EDGE_CURVE('',#6428,#6426,#3776,.T.);
#7949=EDGE_CURVE('',#6429,#6427,#3777,.T.);
#7950=EDGE_CURVE('',#6429,#6430,#3778,.T.);
#7951=EDGE_CURVE('',#6430,#6428,#3779,.T.);
#7952=EDGE_CURVE('',#6420,#6429,#3780,.T.);
#7953=EDGE_CURVE('',#6422,#6430,#3781,.T.);
#7954=EDGE_CURVE('',#6431,#6431,#5493,.T.);
#7955=EDGE_CURVE('',#6432,#6432,#5494,.T.);
#7956=EDGE_CURVE('',#6432,#6431,#3782,.T.);
#7957=EDGE_CURVE('',#6433,#6433,#5495,.F.);
#7958=EDGE_CURVE('',#6433,#6432,#3783,.T.);
#7959=EDGE_CURVE('',#6434,#6434,#5496,.T.);
#7960=EDGE_CURVE('',#6434,#6433,#3784,.T.);
#7961=EDGE_CURVE('',#6435,#6435,#5497,.T.);
#7962=EDGE_CURVE('',#6435,#6436,#3785,.T.);
#7963=EDGE_CURVE('',#6436,#6436,#5498,.T.);
#7964=EDGE_CURVE('',#6437,#6437,#5499,.T.);
#7965=EDGE_CURVE('',#6437,#6438,#3786,.T.);
#7966=EDGE_CURVE('',#6438,#6438,#5500,.T.);
#7967=EDGE_CURVE('',#6439,#6440,#3787,.T.);
#7968=EDGE_CURVE('',#6439,#6441,#3788,.T.);
#7969=EDGE_CURVE('',#6442,#6441,#3789,.T.);
#7970=EDGE_CURVE('',#6442,#6440,#3790,.T.);
#7971=EDGE_CURVE('',#6440,#6443,#5501,.T.);
#7972=EDGE_CURVE('',#6444,#6442,#3791,.T.);
#7973=EDGE_CURVE('',#6443,#6444,#3792,.T.);
#7974=EDGE_CURVE('',#6441,#6445,#3793,.T.);
#7975=EDGE_CURVE('',#6444,#6445,#3794,.T.);
#7976=EDGE_CURVE('',#6443,#6446,#3795,.T.);
#7977=EDGE_CURVE('',#6445,#6446,#3796,.T.);
#7978=EDGE_CURVE('',#6446,#6439,#5502,.T.);
#7979=EDGE_CURVE('',#6447,#6448,#3797,.T.);
#7980=EDGE_CURVE('',#6447,#6449,#3798,.T.);
#7981=EDGE_CURVE('',#6450,#6449,#3799,.T.);
#7982=EDGE_CURVE('',#6450,#6448,#3800,.T.);
#7983=EDGE_CURVE('',#6448,#6451,#5503,.T.);
#7984=EDGE_CURVE('',#6452,#6450,#3801,.T.);
#7985=EDGE_CURVE('',#6451,#6452,#3802,.T.);
#7986=EDGE_CURVE('',#6449,#6453,#3803,.T.);
#7987=EDGE_CURVE('',#6452,#6453,#3804,.T.);
#7988=EDGE_CURVE('',#6451,#6454,#3805,.T.);
#7989=EDGE_CURVE('',#6453,#6454,#3806,.T.);
#7990=EDGE_CURVE('',#6454,#6447,#5504,.T.);
#7991=EDGE_CURVE('',#6455,#6455,#5505,.T.);
#7992=EDGE_CURVE('',#6455,#6456,#3807,.T.);
#7993=EDGE_CURVE('',#6456,#6456,#5506,.T.);
#7994=EDGE_CURVE('',#6457,#6457,#5507,.T.);
#7995=EDGE_CURVE('',#6457,#6458,#3808,.T.);
#7996=EDGE_CURVE('',#6458,#6458,#5508,.T.);
#7997=EDGE_CURVE('',#6459,#6459,#5509,.T.);
#7998=EDGE_CURVE('',#6459,#6460,#3809,.T.);
#7999=EDGE_CURVE('',#6460,#6460,#5510,.T.);
#8000=EDGE_CURVE('',#6461,#6461,#5511,.T.);
#8001=EDGE_CURVE('',#6461,#6462,#3810,.T.);
#8002=EDGE_CURVE('',#6462,#6462,#5512,.T.);
#8003=EDGE_CURVE('',#6463,#6463,#5513,.T.);
#8004=EDGE_CURVE('',#6463,#6464,#3811,.T.);
#8005=EDGE_CURVE('',#6464,#6464,#5514,.T.);
#8006=EDGE_CURVE('',#6465,#6465,#5515,.T.);
#8007=EDGE_CURVE('',#6465,#6466,#3812,.T.);
#8008=EDGE_CURVE('',#6466,#6466,#5516,.T.);
#8009=EDGE_CURVE('',#6467,#6467,#5517,.T.);
#8010=EDGE_CURVE('',#6467,#6468,#3813,.T.);
#8011=EDGE_CURVE('',#6468,#6468,#5518,.T.);
#8012=EDGE_CURVE('',#6469,#6469,#5519,.T.);
#8013=EDGE_CURVE('',#6469,#6470,#3814,.T.);
#8014=EDGE_CURVE('',#6470,#6470,#5520,.T.);
#8015=EDGE_CURVE('',#6471,#6471,#5521,.T.);
#8016=EDGE_CURVE('',#6471,#6472,#3815,.T.);
#8017=EDGE_CURVE('',#6472,#6472,#5522,.T.);
#8018=EDGE_CURVE('',#6473,#6474,#3816,.T.);
#8019=EDGE_CURVE('',#6474,#6475,#3817,.T.);
#8020=EDGE_CURVE('',#6476,#6475,#3818,.T.);
#8021=EDGE_CURVE('',#6473,#6476,#3819,.T.);
#8022=EDGE_CURVE('',#6477,#6473,#3820,.T.);
#8023=EDGE_CURVE('',#6478,#6476,#3821,.T.);
#8024=EDGE_CURVE('',#6477,#6478,#3822,.T.);
#8025=EDGE_CURVE('',#6479,#6477,#3823,.T.);
#8026=EDGE_CURVE('',#6480,#6478,#3824,.T.);
#8027=EDGE_CURVE('',#6479,#6480,#3825,.T.);
#8028=EDGE_CURVE('',#6474,#6479,#3826,.T.);
#8029=EDGE_CURVE('',#6475,#6480,#3827,.T.);
#8030=EDGE_CURVE('',#6481,#6482,#3828,.T.);
#8031=EDGE_CURVE('',#6482,#6483,#3829,.T.);
#8032=EDGE_CURVE('',#6484,#6483,#3830,.T.);
#8033=EDGE_CURVE('',#6481,#6484,#3831,.T.);
#8034=EDGE_CURVE('',#6485,#6481,#3832,.T.);
#8035=EDGE_CURVE('',#6486,#6484,#3833,.T.);
#8036=EDGE_CURVE('',#6485,#6486,#3834,.T.);
#8037=EDGE_CURVE('',#6487,#6485,#3835,.T.);
#8038=EDGE_CURVE('',#6488,#6486,#3836,.T.);
#8039=EDGE_CURVE('',#6487,#6488,#3837,.T.);
#8040=EDGE_CURVE('',#6482,#6487,#3838,.T.);
#8041=EDGE_CURVE('',#6483,#6488,#3839,.T.);
#8042=EDGE_CURVE('',#6489,#6489,#5523,.T.);
#8043=EDGE_CURVE('',#6489,#6490,#3840,.T.);
#8044=EDGE_CURVE('',#6490,#6490,#5524,.T.);
#8045=EDGE_CURVE('',#6491,#6492,#3841,.T.);
#8046=EDGE_CURVE('',#6491,#6493,#3842,.T.);
#8047=EDGE_CURVE('',#6494,#6493,#3843,.T.);
#8048=EDGE_CURVE('',#6492,#6494,#3844,.T.);
#8049=EDGE_CURVE('',#6495,#6491,#3845,.T.);
#8050=EDGE_CURVE('',#6495,#6496,#3846,.T.);
#8051=EDGE_CURVE('',#6493,#6496,#3847,.T.);
#8052=EDGE_CURVE('',#6497,#6495,#3848,.T.);
#8053=EDGE_CURVE('',#6498,#6497,#3849,.T.);
#8054=EDGE_CURVE('',#6496,#6498,#3850,.T.);
#8055=EDGE_CURVE('',#6499,#6499,#5525,.T.);
#8056=EDGE_CURVE('',#6498,#6494,#5526,.T.);
#8057=EDGE_CURVE('',#6497,#6492,#5527,.T.);
#8058=EDGE_CURVE('',#6500,#6501,#3851,.T.);
#8059=EDGE_CURVE('',#6502,#6500,#5528,.T.);
#8060=EDGE_CURVE('',#6503,#6502,#3852,.T.);
#8061=EDGE_CURVE('',#6503,#6501,#5529,.T.);
#8062=EDGE_CURVE('',#6504,#6501,#3853,.T.);
#8063=EDGE_CURVE('',#6505,#6504,#3854,.T.);
#8064=EDGE_CURVE('',#6500,#6505,#3855,.T.);
#8065=EDGE_CURVE('',#6503,#6506,#3856,.T.);
#8066=EDGE_CURVE('',#6504,#6506,#5530,.T.);
#8067=EDGE_CURVE('',#6507,#6502,#3857,.T.);
#8068=EDGE_CURVE('',#6506,#6507,#3858,.T.);
#8069=EDGE_CURVE('',#6507,#6505,#5531,.T.);
#8070=EDGE_CURVE('',#6499,#6508,#3859,.T.);
#8071=EDGE_CURVE('',#6508,#6508,#5532,.T.);
#8072=EDGE_CURVE('',#6509,#6509,#5533,.T.);
#8073=EDGE_CURVE('',#6509,#6510,#3860,.T.);
#8074=EDGE_CURVE('',#6510,#6510,#5534,.T.);
#8075=EDGE_CURVE('',#6511,#6511,#5535,.T.);
#8076=EDGE_CURVE('',#6511,#6512,#3861,.T.);
#8077=EDGE_CURVE('',#6512,#6512,#5536,.T.);
#8078=EDGE_CURVE('',#6513,#6513,#5537,.T.);
#8079=EDGE_CURVE('',#6513,#6514,#3862,.T.);
#8080=EDGE_CURVE('',#6514,#6514,#5538,.T.);
#8081=EDGE_CURVE('',#6515,#6515,#5539,.T.);
#8082=EDGE_CURVE('',#6515,#6516,#3863,.T.);
#8083=EDGE_CURVE('',#6516,#6516,#5540,.T.);
#8084=EDGE_CURVE('',#6517,#6517,#5541,.T.);
#8085=EDGE_CURVE('',#6517,#6518,#3864,.T.);
#8086=EDGE_CURVE('',#6518,#6518,#5542,.T.);
#8087=EDGE_CURVE('',#6519,#6519,#5543,.T.);
#8088=EDGE_CURVE('',#6519,#6520,#3865,.T.);
#8089=EDGE_CURVE('',#6520,#6520,#5544,.T.);
#8090=EDGE_CURVE('',#6521,#6522,#3866,.T.);
#8091=EDGE_CURVE('',#6523,#6521,#3867,.T.);
#8092=EDGE_CURVE('',#6524,#6523,#3868,.T.);
#8093=EDGE_CURVE('',#6522,#6524,#3869,.T.);
#8094=EDGE_CURVE('',#6525,#6521,#3870,.T.);
#8095=EDGE_CURVE('',#6525,#6526,#3871,.T.);
#8096=EDGE_CURVE('',#6523,#6526,#3872,.T.);
#8097=EDGE_CURVE('',#6527,#6525,#3873,.T.);
#8098=EDGE_CURVE('',#6528,#6527,#3874,.T.);
#8099=EDGE_CURVE('',#6526,#6528,#3875,.T.);
#8100=EDGE_CURVE('',#6529,#6530,#5545,.T.);
#8101=EDGE_CURVE('',#6530,#6531,#51,.T.);
#8102=EDGE_CURVE('',#6531,#6532,#3876,.T.);
#8103=EDGE_CURVE('',#6532,#6533,#52,.T.);
#8104=EDGE_CURVE('',#6533,#6534,#5546,.T.);
#8105=EDGE_CURVE('',#6534,#6535,#53,.T.);
#8106=EDGE_CURVE('',#6535,#6536,#3877,.T.);
#8107=EDGE_CURVE('',#6536,#6537,#54,.T.);
#8108=EDGE_CURVE('',#6537,#6538,#5547,.T.);
#8109=EDGE_CURVE('',#6538,#6539,#55,.T.);
#8110=EDGE_CURVE('',#6539,#6540,#3878,.T.);
#8111=EDGE_CURVE('',#6540,#6541,#56,.T.);
#8112=EDGE_CURVE('',#6541,#6542,#5548,.T.);
#8113=EDGE_CURVE('',#6542,#6543,#57,.T.);
#8114=EDGE_CURVE('',#6543,#6544,#3879,.T.);
#8115=EDGE_CURVE('',#6544,#6545,#58,.T.);
#8116=EDGE_CURVE('',#6545,#6546,#5549,.T.);
#8117=EDGE_CURVE('',#6546,#6547,#59,.T.);
#8118=EDGE_CURVE('',#6547,#6548,#3880,.T.);
#8119=EDGE_CURVE('',#6548,#6549,#60,.T.);
#8120=EDGE_CURVE('',#6549,#6550,#5550,.T.);
#8121=EDGE_CURVE('',#6550,#6551,#61,.T.);
#8122=EDGE_CURVE('',#6551,#6552,#3881,.T.);
#8123=EDGE_CURVE('',#6552,#6553,#62,.T.);
#8124=EDGE_CURVE('',#6553,#6554,#5551,.T.);
#8125=EDGE_CURVE('',#6554,#6555,#63,.T.);
#8126=EDGE_CURVE('',#6555,#6556,#3882,.T.);
#8127=EDGE_CURVE('',#6556,#6557,#64,.T.);
#8128=EDGE_CURVE('',#6557,#6558,#5552,.T.);
#8129=EDGE_CURVE('',#6558,#6559,#65,.T.);
#8130=EDGE_CURVE('',#6559,#6560,#3883,.T.);
#8131=EDGE_CURVE('',#6560,#6561,#66,.T.);
#8132=EDGE_CURVE('',#6561,#6562,#5553,.T.);
#8133=EDGE_CURVE('',#6562,#6563,#67,.T.);
#8134=EDGE_CURVE('',#6563,#6564,#3884,.T.);
#8135=EDGE_CURVE('',#6564,#6565,#68,.T.);
#8136=EDGE_CURVE('',#6565,#6566,#5554,.T.);
#8137=EDGE_CURVE('',#6566,#6567,#69,.T.);
#8138=EDGE_CURVE('',#6567,#6568,#3885,.T.);
#8139=EDGE_CURVE('',#6568,#6569,#70,.T.);
#8140=EDGE_CURVE('',#6569,#6570,#5555,.T.);
#8141=EDGE_CURVE('',#6570,#6571,#71,.T.);
#8142=EDGE_CURVE('',#6571,#6572,#3886,.T.);
#8143=EDGE_CURVE('',#6572,#6573,#72,.T.);
#8144=EDGE_CURVE('',#6573,#6574,#5556,.T.);
#8145=EDGE_CURVE('',#6574,#6575,#73,.T.);
#8146=EDGE_CURVE('',#6575,#6576,#3887,.T.);
#8147=EDGE_CURVE('',#6576,#6577,#74,.T.);
#8148=EDGE_CURVE('',#6577,#6578,#5557,.T.);
#8149=EDGE_CURVE('',#6578,#6579,#75,.T.);
#8150=EDGE_CURVE('',#6579,#6580,#3888,.T.);
#8151=EDGE_CURVE('',#6580,#6581,#76,.T.);
#8152=EDGE_CURVE('',#6581,#6582,#5558,.T.);
#8153=EDGE_CURVE('',#6582,#6583,#77,.T.);
#8154=EDGE_CURVE('',#6583,#6584,#3889,.T.);
#8155=EDGE_CURVE('',#6584,#6585,#78,.T.);
#8156=EDGE_CURVE('',#6585,#6586,#5559,.T.);
#8157=EDGE_CURVE('',#6586,#6587,#79,.T.);
#8158=EDGE_CURVE('',#6587,#6588,#3890,.T.);
#8159=EDGE_CURVE('',#6588,#6589,#80,.T.);
#8160=EDGE_CURVE('',#6589,#6590,#5560,.T.);
#8161=EDGE_CURVE('',#6590,#6591,#81,.T.);
#8162=EDGE_CURVE('',#6591,#6592,#3891,.T.);
#8163=EDGE_CURVE('',#6592,#6593,#82,.T.);
#8164=EDGE_CURVE('',#6593,#6594,#5561,.T.);
#8165=EDGE_CURVE('',#6594,#6595,#83,.T.);
#8166=EDGE_CURVE('',#6595,#6596,#3892,.T.);
#8167=EDGE_CURVE('',#6596,#6597,#84,.T.);
#8168=EDGE_CURVE('',#6597,#6598,#5562,.T.);
#8169=EDGE_CURVE('',#6598,#6599,#85,.T.);
#8170=EDGE_CURVE('',#6599,#6600,#3893,.T.);
#8171=EDGE_CURVE('',#6600,#6601,#86,.T.);
#8172=EDGE_CURVE('',#6601,#6602,#5563,.T.);
#8173=EDGE_CURVE('',#6602,#6603,#87,.T.);
#8174=EDGE_CURVE('',#6603,#6604,#3894,.T.);
#8175=EDGE_CURVE('',#6604,#6605,#88,.T.);
#8176=EDGE_CURVE('',#6605,#6606,#5564,.T.);
#8177=EDGE_CURVE('',#6606,#6607,#89,.T.);
#8178=EDGE_CURVE('',#6607,#6608,#3895,.T.);
#8179=EDGE_CURVE('',#6608,#6529,#90,.T.);
#8180=EDGE_CURVE('',#6528,#6524,#5565,.T.);
#8181=EDGE_CURVE('',#6522,#6527,#5566,.T.);
#8182=EDGE_CURVE('',#6609,#6609,#5567,.T.);
#8183=EDGE_CURVE('',#6609,#6610,#3896,.T.);
#8184=EDGE_CURVE('',#6610,#6610,#5568,.T.);
#8185=EDGE_CURVE('',#6611,#6606,#3897,.T.);
#8186=EDGE_CURVE('',#6612,#6611,#91,.T.);
#8187=EDGE_CURVE('',#6607,#6612,#3898,.T.);
#8188=EDGE_CURVE('',#6613,#6612,#3899,.T.);
#8189=EDGE_CURVE('',#6608,#6613,#3900,.T.);
#8190=EDGE_CURVE('',#6614,#6613,#92,.T.);
#8191=EDGE_CURVE('',#6529,#6614,#3901,.T.);
#8192=EDGE_CURVE('',#6615,#6614,#5569,.T.);
#8193=EDGE_CURVE('',#6615,#6530,#3902,.T.);
#8194=EDGE_CURVE('',#6616,#6615,#93,.T.);
#8195=EDGE_CURVE('',#6531,#6616,#3903,.T.);
#8196=EDGE_CURVE('',#6617,#6616,#3904,.T.);
#8197=EDGE_CURVE('',#6532,#6617,#3905,.T.);
#8198=EDGE_CURVE('',#6618,#6617,#94,.T.);
#8199=EDGE_CURVE('',#6533,#6618,#3906,.T.);
#8200=EDGE_CURVE('',#6619,#6618,#5570,.T.);
#8201=EDGE_CURVE('',#6619,#6534,#3907,.T.);
#8202=EDGE_CURVE('',#6620,#6619,#95,.T.);
#8203=EDGE_CURVE('',#6535,#6620,#3908,.T.);
#8204=EDGE_CURVE('',#6621,#6620,#3909,.T.);
#8205=EDGE_CURVE('',#6536,#6621,#3910,.T.);
#8206=EDGE_CURVE('',#6622,#6621,#96,.T.);
#8207=EDGE_CURVE('',#6537,#6622,#3911,.T.);
#8208=EDGE_CURVE('',#6623,#6622,#5571,.T.);
#8209=EDGE_CURVE('',#6623,#6538,#3912,.T.);
#8210=EDGE_CURVE('',#6624,#6623,#97,.T.);
#8211=EDGE_CURVE('',#6539,#6624,#3913,.T.);
#8212=EDGE_CURVE('',#6625,#6624,#3914,.T.);
#8213=EDGE_CURVE('',#6540,#6625,#3915,.T.);
#8214=EDGE_CURVE('',#6626,#6625,#98,.T.);
#8215=EDGE_CURVE('',#6541,#6626,#3916,.T.);
#8216=EDGE_CURVE('',#6627,#6626,#5572,.T.);
#8217=EDGE_CURVE('',#6627,#6542,#3917,.T.);
#8218=EDGE_CURVE('',#6628,#6627,#99,.T.);
#8219=EDGE_CURVE('',#6543,#6628,#3918,.T.);
#8220=EDGE_CURVE('',#6629,#6628,#3919,.T.);
#8221=EDGE_CURVE('',#6544,#6629,#3920,.T.);
#8222=EDGE_CURVE('',#6630,#6629,#100,.T.);
#8223=EDGE_CURVE('',#6545,#6630,#3921,.T.);
#8224=EDGE_CURVE('',#6631,#6630,#5573,.T.);
#8225=EDGE_CURVE('',#6631,#6546,#3922,.T.);
#8226=EDGE_CURVE('',#6632,#6631,#101,.T.);
#8227=EDGE_CURVE('',#6547,#6632,#3923,.T.);
#8228=EDGE_CURVE('',#6633,#6632,#3924,.T.);
#8229=EDGE_CURVE('',#6548,#6633,#3925,.T.);
#8230=EDGE_CURVE('',#6634,#6633,#102,.T.);
#8231=EDGE_CURVE('',#6549,#6634,#3926,.T.);
#8232=EDGE_CURVE('',#6635,#6634,#5574,.T.);
#8233=EDGE_CURVE('',#6635,#6550,#3927,.T.);
#8234=EDGE_CURVE('',#6636,#6635,#103,.T.);
#8235=EDGE_CURVE('',#6551,#6636,#3928,.T.);
#8236=EDGE_CURVE('',#6637,#6636,#3929,.T.);
#8237=EDGE_CURVE('',#6552,#6637,#3930,.T.);
#8238=EDGE_CURVE('',#6638,#6637,#104,.T.);
#8239=EDGE_CURVE('',#6553,#6638,#3931,.T.);
#8240=EDGE_CURVE('',#6639,#6638,#5575,.T.);
#8241=EDGE_CURVE('',#6639,#6554,#3932,.T.);
#8242=EDGE_CURVE('',#6640,#6639,#105,.T.);
#8243=EDGE_CURVE('',#6555,#6640,#3933,.T.);
#8244=EDGE_CURVE('',#6641,#6640,#3934,.T.);
#8245=EDGE_CURVE('',#6556,#6641,#3935,.T.);
#8246=EDGE_CURVE('',#6642,#6641,#106,.T.);
#8247=EDGE_CURVE('',#6557,#6642,#3936,.T.);
#8248=EDGE_CURVE('',#6643,#6642,#5576,.T.);
#8249=EDGE_CURVE('',#6643,#6558,#3937,.T.);
#8250=EDGE_CURVE('',#6644,#6643,#107,.T.);
#8251=EDGE_CURVE('',#6559,#6644,#3938,.T.);
#8252=EDGE_CURVE('',#6645,#6644,#3939,.T.);
#8253=EDGE_CURVE('',#6560,#6645,#3940,.T.);
#8254=EDGE_CURVE('',#6646,#6645,#108,.T.);
#8255=EDGE_CURVE('',#6561,#6646,#3941,.T.);
#8256=EDGE_CURVE('',#6647,#6646,#5577,.T.);
#8257=EDGE_CURVE('',#6647,#6562,#3942,.T.);
#8258=EDGE_CURVE('',#6648,#6647,#109,.T.);
#8259=EDGE_CURVE('',#6563,#6648,#3943,.T.);
#8260=EDGE_CURVE('',#6649,#6648,#3944,.T.);
#8261=EDGE_CURVE('',#6564,#6649,#3945,.T.);
#8262=EDGE_CURVE('',#6650,#6649,#110,.T.);
#8263=EDGE_CURVE('',#6565,#6650,#3946,.T.);
#8264=EDGE_CURVE('',#6651,#6650,#5578,.T.);
#8265=EDGE_CURVE('',#6651,#6566,#3947,.T.);
#8266=EDGE_CURVE('',#6652,#6651,#111,.T.);
#8267=EDGE_CURVE('',#6567,#6652,#3948,.T.);
#8268=EDGE_CURVE('',#6653,#6652,#3949,.T.);
#8269=EDGE_CURVE('',#6568,#6653,#3950,.T.);
#8270=EDGE_CURVE('',#6654,#6653,#112,.T.);
#8271=EDGE_CURVE('',#6569,#6654,#3951,.T.);
#8272=EDGE_CURVE('',#6655,#6654,#5579,.T.);
#8273=EDGE_CURVE('',#6655,#6570,#3952,.T.);
#8274=EDGE_CURVE('',#6656,#6655,#113,.T.);
#8275=EDGE_CURVE('',#6571,#6656,#3953,.T.);
#8276=EDGE_CURVE('',#6657,#6656,#3954,.T.);
#8277=EDGE_CURVE('',#6572,#6657,#3955,.T.);
#8278=EDGE_CURVE('',#6658,#6657,#114,.T.);
#8279=EDGE_CURVE('',#6573,#6658,#3956,.T.);
#8280=EDGE_CURVE('',#6659,#6658,#5580,.T.);
#8281=EDGE_CURVE('',#6659,#6574,#3957,.T.);
#8282=EDGE_CURVE('',#6660,#6659,#115,.T.);
#8283=EDGE_CURVE('',#6575,#6660,#3958,.T.);
#8284=EDGE_CURVE('',#6661,#6660,#3959,.T.);
#8285=EDGE_CURVE('',#6576,#6661,#3960,.T.);
#8286=EDGE_CURVE('',#6662,#6661,#116,.T.);
#8287=EDGE_CURVE('',#6577,#6662,#3961,.T.);
#8288=EDGE_CURVE('',#6663,#6662,#5581,.T.);
#8289=EDGE_CURVE('',#6663,#6578,#3962,.T.);
#8290=EDGE_CURVE('',#6664,#6663,#117,.T.);
#8291=EDGE_CURVE('',#6579,#6664,#3963,.T.);
#8292=EDGE_CURVE('',#6665,#6664,#3964,.T.);
#8293=EDGE_CURVE('',#6580,#6665,#3965,.T.);
#8294=EDGE_CURVE('',#6666,#6665,#118,.T.);
#8295=EDGE_CURVE('',#6581,#6666,#3966,.T.);
#8296=EDGE_CURVE('',#6667,#6666,#5582,.T.);
#8297=EDGE_CURVE('',#6667,#6582,#3967,.T.);
#8298=EDGE_CURVE('',#6668,#6667,#119,.T.);
#8299=EDGE_CURVE('',#6583,#6668,#3968,.T.);
#8300=EDGE_CURVE('',#6669,#6668,#3969,.T.);
#8301=EDGE_CURVE('',#6584,#6669,#3970,.T.);
#8302=EDGE_CURVE('',#6670,#6669,#120,.T.);
#8303=EDGE_CURVE('',#6585,#6670,#3971,.T.);
#8304=EDGE_CURVE('',#6671,#6670,#5583,.T.);
#8305=EDGE_CURVE('',#6671,#6586,#3972,.T.);
#8306=EDGE_CURVE('',#6672,#6671,#121,.T.);
#8307=EDGE_CURVE('',#6587,#6672,#3973,.T.);
#8308=EDGE_CURVE('',#6673,#6672,#3974,.T.);
#8309=EDGE_CURVE('',#6588,#6673,#3975,.T.);
#8310=EDGE_CURVE('',#6674,#6673,#122,.T.);
#8311=EDGE_CURVE('',#6589,#6674,#3976,.T.);
#8312=EDGE_CURVE('',#6675,#6674,#5584,.T.);
#8313=EDGE_CURVE('',#6675,#6590,#3977,.T.);
#8314=EDGE_CURVE('',#6676,#6675,#123,.T.);
#8315=EDGE_CURVE('',#6591,#6676,#3978,.T.);
#8316=EDGE_CURVE('',#6677,#6676,#3979,.T.);
#8317=EDGE_CURVE('',#6592,#6677,#3980,.T.);
#8318=EDGE_CURVE('',#6678,#6677,#124,.T.);
#8319=EDGE_CURVE('',#6593,#6678,#3981,.T.);
#8320=EDGE_CURVE('',#6679,#6678,#5585,.T.);
#8321=EDGE_CURVE('',#6679,#6594,#3982,.T.);
#8322=EDGE_CURVE('',#6680,#6679,#125,.T.);
#8323=EDGE_CURVE('',#6595,#6680,#3983,.T.);
#8324=EDGE_CURVE('',#6681,#6680,#3984,.T.);
#8325=EDGE_CURVE('',#6596,#6681,#3985,.T.);
#8326=EDGE_CURVE('',#6682,#6681,#126,.T.);
#8327=EDGE_CURVE('',#6597,#6682,#3986,.T.);
#8328=EDGE_CURVE('',#6683,#6682,#5586,.T.);
#8329=EDGE_CURVE('',#6683,#6598,#3987,.T.);
#8330=EDGE_CURVE('',#6684,#6683,#127,.T.);
#8331=EDGE_CURVE('',#6599,#6684,#3988,.T.);
#8332=EDGE_CURVE('',#6685,#6684,#3989,.T.);
#8333=EDGE_CURVE('',#6600,#6685,#3990,.T.);
#8334=EDGE_CURVE('',#6686,#6685,#128,.T.);
#8335=EDGE_CURVE('',#6601,#6686,#3991,.T.);
#8336=EDGE_CURVE('',#6687,#6686,#5587,.T.);
#8337=EDGE_CURVE('',#6687,#6602,#3992,.T.);
#8338=EDGE_CURVE('',#6688,#6687,#129,.T.);
#8339=EDGE_CURVE('',#6603,#6688,#3993,.T.);
#8340=EDGE_CURVE('',#6689,#6688,#3994,.T.);
#8341=EDGE_CURVE('',#6604,#6689,#3995,.T.);
#8342=EDGE_CURVE('',#6690,#6689,#130,.T.);
#8343=EDGE_CURVE('',#6605,#6690,#3996,.T.);
#8344=EDGE_CURVE('',#6611,#6690,#5588,.T.);
#8345=EDGE_CURVE('',#6691,#6691,#5589,.T.);
#8346=EDGE_CURVE('',#6691,#6692,#3997,.T.);
#8347=EDGE_CURVE('',#6692,#6692,#5590,.T.);
#8348=EDGE_CURVE('',#6693,#6693,#5591,.T.);
#8349=EDGE_CURVE('',#6693,#6694,#3998,.T.);
#8350=EDGE_CURVE('',#6694,#6694,#5592,.T.);
#8351=EDGE_CURVE('',#6695,#6695,#5593,.T.);
#8352=EDGE_CURVE('',#6696,#6696,#5594,.T.);
#8353=EDGE_CURVE('',#6696,#6695,#3999,.T.);
#8354=EDGE_CURVE('',#6697,#6697,#5595,.T.);
#8355=EDGE_CURVE('',#6697,#6696,#4000,.T.);
#8356=EDGE_CURVE('',#6698,#6698,#5596,.T.);
#8357=EDGE_CURVE('',#6698,#6697,#4001,.T.);
#8358=EDGE_CURVE('',#6699,#6699,#5597,.T.);
#8359=EDGE_CURVE('',#6700,#6700,#5598,.F.);
#8360=EDGE_CURVE('',#6700,#6699,#4002,.T.);
#8361=EDGE_CURVE('',#6701,#6701,#5599,.F.);
#8362=EDGE_CURVE('',#6701,#6700,#4003,.T.);
#8363=EDGE_CURVE('',#6702,#6702,#5600,.T.);
#8364=EDGE_CURVE('',#6702,#6701,#4004,.T.);
#8365=EDGE_CURVE('',#6703,#6704,#4005,.T.);
#8366=EDGE_CURVE('',#6704,#6705,#4006,.T.);
#8367=EDGE_CURVE('',#6705,#6706,#4007,.T.);
#8368=EDGE_CURVE('',#6703,#6706,#4008,.T.);
#8369=EDGE_CURVE('',#6704,#6707,#4009,.T.);
#8370=EDGE_CURVE('',#6707,#6708,#4010,.T.);
#8371=EDGE_CURVE('',#6708,#6705,#4011,.T.);
#8372=EDGE_CURVE('',#6707,#6709,#4012,.T.);
#8373=EDGE_CURVE('',#6709,#6710,#4013,.T.);
#8374=EDGE_CURVE('',#6710,#6708,#4014,.T.);
#8375=EDGE_CURVE('',#6709,#6711,#4015,.T.);
#8376=EDGE_CURVE('',#6711,#6712,#4016,.T.);
#8377=EDGE_CURVE('',#6712,#6710,#4017,.T.);
#8378=EDGE_CURVE('',#6711,#6713,#4018,.T.);
#8379=EDGE_CURVE('',#6713,#6714,#4019,.T.);
#8380=EDGE_CURVE('',#6714,#6712,#4020,.T.);
#8381=EDGE_CURVE('',#6713,#6703,#4021,.T.);
#8382=EDGE_CURVE('',#6706,#6714,#4022,.T.);
#8383=EDGE_CURVE('',#6715,#6715,#5601,.T.);
#8384=EDGE_CURVE('',#6716,#6716,#5602,.T.);
#8385=EDGE_CURVE('',#6716,#6715,#4023,.T.);
#8386=EDGE_CURVE('',#6717,#6717,#5603,.T.);
#8387=EDGE_CURVE('',#6717,#6716,#4024,.T.);
#8388=EDGE_CURVE('',#6718,#6718,#5604,.T.);
#8389=EDGE_CURVE('',#6718,#6717,#4025,.T.);
#8390=EDGE_CURVE('',#6719,#6719,#5605,.T.);
#8391=EDGE_CURVE('',#6720,#6720,#5606,.F.);
#8392=EDGE_CURVE('',#6720,#6719,#4026,.T.);
#8393=EDGE_CURVE('',#6721,#6721,#5607,.F.);
#8394=EDGE_CURVE('',#6721,#6720,#4027,.T.);
#8395=EDGE_CURVE('',#6722,#6722,#5608,.T.);
#8396=EDGE_CURVE('',#6722,#6721,#4028,.T.);
#8397=EDGE_CURVE('',#6723,#6724,#4029,.T.);
#8398=EDGE_CURVE('',#6724,#6725,#4030,.T.);
#8399=EDGE_CURVE('',#6725,#6726,#4031,.T.);
#8400=EDGE_CURVE('',#6723,#6726,#4032,.T.);
#8401=EDGE_CURVE('',#6724,#6727,#4033,.T.);
#8402=EDGE_CURVE('',#6727,#6728,#4034,.T.);
#8403=EDGE_CURVE('',#6728,#6725,#4035,.T.);
#8404=EDGE_CURVE('',#6727,#6729,#4036,.T.);
#8405=EDGE_CURVE('',#6729,#6730,#4037,.T.);
#8406=EDGE_CURVE('',#6730,#6728,#4038,.T.);
#8407=EDGE_CURVE('',#6729,#6731,#4039,.T.);
#8408=EDGE_CURVE('',#6731,#6732,#4040,.T.);
#8409=EDGE_CURVE('',#6732,#6730,#4041,.T.);
#8410=EDGE_CURVE('',#6731,#6733,#4042,.T.);
#8411=EDGE_CURVE('',#6733,#6734,#4043,.T.);
#8412=EDGE_CURVE('',#6734,#6732,#4044,.T.);
#8413=EDGE_CURVE('',#6733,#6723,#4045,.T.);
#8414=EDGE_CURVE('',#6726,#6734,#4046,.T.);
#8415=EDGE_CURVE('',#6735,#6735,#5609,.T.);
#8416=EDGE_CURVE('',#6735,#6736,#4047,.T.);
#8417=EDGE_CURVE('',#6736,#6736,#5610,.T.);
#8418=EDGE_CURVE('',#6737,#6737,#5611,.T.);
#8419=EDGE_CURVE('',#6737,#6738,#4048,.T.);
#8420=EDGE_CURVE('',#6738,#6738,#5612,.T.);
#8421=ORIENTED_EDGE('',*,*,#6739,.F.);
#8422=ORIENTED_EDGE('',*,*,#6740,.T.);
#8423=ORIENTED_EDGE('',*,*,#6741,.F.);
#8424=ORIENTED_EDGE('',*,*,#6740,.F.);
#8425=ORIENTED_EDGE('',*,*,#6742,.F.);
#8426=ORIENTED_EDGE('',*,*,#6743,.T.);
#8427=ORIENTED_EDGE('',*,*,#6744,.F.);
#8428=ORIENTED_EDGE('',*,*,#6743,.F.);
#8429=ORIENTED_EDGE('',*,*,#6745,.F.);
#8430=ORIENTED_EDGE('',*,*,#6746,.T.);
#8431=ORIENTED_EDGE('',*,*,#6747,.F.);
#8432=ORIENTED_EDGE('',*,*,#6746,.F.);
#8433=ORIENTED_EDGE('',*,*,#6748,.F.);
#8434=ORIENTED_EDGE('',*,*,#6749,.T.);
#8435=ORIENTED_EDGE('',*,*,#6750,.F.);
#8436=ORIENTED_EDGE('',*,*,#6749,.F.);
#8437=ORIENTED_EDGE('',*,*,#6751,.F.);
#8438=ORIENTED_EDGE('',*,*,#6752,.T.);
#8439=ORIENTED_EDGE('',*,*,#6753,.F.);
#8440=ORIENTED_EDGE('',*,*,#6752,.F.);
#8441=ORIENTED_EDGE('',*,*,#6754,.F.);
#8442=ORIENTED_EDGE('',*,*,#6755,.T.);
#8443=ORIENTED_EDGE('',*,*,#6756,.F.);
#8444=ORIENTED_EDGE('',*,*,#6755,.F.);
#8445=ORIENTED_EDGE('',*,*,#6757,.T.);
#8446=ORIENTED_EDGE('',*,*,#6758,.T.);
#8447=ORIENTED_EDGE('',*,*,#6759,.F.);
#8448=ORIENTED_EDGE('',*,*,#6760,.F.);
#8449=ORIENTED_EDGE('',*,*,#6761,.T.);
#8450=ORIENTED_EDGE('',*,*,#6760,.T.);
#8451=ORIENTED_EDGE('',*,*,#6762,.F.);
#8452=ORIENTED_EDGE('',*,*,#6763,.F.);
#8453=ORIENTED_EDGE('',*,*,#6764,.T.);
#8454=ORIENTED_EDGE('',*,*,#6763,.T.);
#8455=ORIENTED_EDGE('',*,*,#6765,.F.);
#8456=ORIENTED_EDGE('',*,*,#6766,.F.);
#8457=ORIENTED_EDGE('',*,*,#6767,.T.);
#8458=ORIENTED_EDGE('',*,*,#6766,.T.);
#8459=ORIENTED_EDGE('',*,*,#6768,.F.);
#8460=ORIENTED_EDGE('',*,*,#6758,.F.);
#8461=ORIENTED_EDGE('',*,*,#6768,.T.);
#8462=ORIENTED_EDGE('',*,*,#6765,.T.);
#8463=ORIENTED_EDGE('',*,*,#6762,.T.);
#8464=ORIENTED_EDGE('',*,*,#6759,.T.);
#8465=ORIENTED_EDGE('',*,*,#6741,.T.);
#8466=ORIENTED_EDGE('',*,*,#6744,.T.);
#8467=ORIENTED_EDGE('',*,*,#6747,.T.);
#8468=ORIENTED_EDGE('',*,*,#6750,.T.);
#8469=ORIENTED_EDGE('',*,*,#6753,.T.);
#8470=ORIENTED_EDGE('',*,*,#6756,.T.);
#8471=ORIENTED_EDGE('',*,*,#6767,.F.);
#8472=ORIENTED_EDGE('',*,*,#6757,.F.);
#8473=ORIENTED_EDGE('',*,*,#6761,.F.);
#8474=ORIENTED_EDGE('',*,*,#6764,.F.);
#8475=ORIENTED_EDGE('',*,*,#6739,.T.);
#8476=ORIENTED_EDGE('',*,*,#6742,.T.);
#8477=ORIENTED_EDGE('',*,*,#6745,.T.);
#8478=ORIENTED_EDGE('',*,*,#6748,.T.);
#8479=ORIENTED_EDGE('',*,*,#6751,.T.);
#8480=ORIENTED_EDGE('',*,*,#6754,.T.);
#8481=ORIENTED_EDGE('',*,*,#6769,.T.);
#8482=ORIENTED_EDGE('',*,*,#6770,.T.);
#8483=ORIENTED_EDGE('',*,*,#6771,.F.);
#8484=ORIENTED_EDGE('',*,*,#6772,.F.);
#8485=ORIENTED_EDGE('',*,*,#6773,.T.);
#8486=ORIENTED_EDGE('',*,*,#6772,.T.);
#8487=ORIENTED_EDGE('',*,*,#6774,.F.);
#8488=ORIENTED_EDGE('',*,*,#6775,.F.);
#8489=ORIENTED_EDGE('',*,*,#6776,.T.);
#8490=ORIENTED_EDGE('',*,*,#6775,.T.);
#8491=ORIENTED_EDGE('',*,*,#6777,.F.);
#8492=ORIENTED_EDGE('',*,*,#6778,.F.);
#8493=ORIENTED_EDGE('',*,*,#6779,.T.);
#8494=ORIENTED_EDGE('',*,*,#6778,.T.);
#8495=ORIENTED_EDGE('',*,*,#6780,.F.);
#8496=ORIENTED_EDGE('',*,*,#6770,.F.);
#8497=ORIENTED_EDGE('',*,*,#6780,.T.);
#8498=ORIENTED_EDGE('',*,*,#6777,.T.);
#8499=ORIENTED_EDGE('',*,*,#6774,.T.);
#8500=ORIENTED_EDGE('',*,*,#6771,.T.);
#8501=ORIENTED_EDGE('',*,*,#6779,.F.);
#8502=ORIENTED_EDGE('',*,*,#6769,.F.);
#8503=ORIENTED_EDGE('',*,*,#6773,.F.);
#8504=ORIENTED_EDGE('',*,*,#6776,.F.);
#8505=ORIENTED_EDGE('',*,*,#6781,.T.);
#8506=ORIENTED_EDGE('',*,*,#6782,.T.);
#8507=ORIENTED_EDGE('',*,*,#6783,.F.);
#8508=ORIENTED_EDGE('',*,*,#6784,.F.);
#8509=ORIENTED_EDGE('',*,*,#6785,.T.);
#8510=ORIENTED_EDGE('',*,*,#6784,.T.);
#8511=ORIENTED_EDGE('',*,*,#6786,.F.);
#8512=ORIENTED_EDGE('',*,*,#6787,.F.);
#8513=ORIENTED_EDGE('',*,*,#6788,.T.);
#8514=ORIENTED_EDGE('',*,*,#6787,.T.);
#8515=ORIENTED_EDGE('',*,*,#6789,.F.);
#8516=ORIENTED_EDGE('',*,*,#6790,.F.);
#8517=ORIENTED_EDGE('',*,*,#6791,.T.);
#8518=ORIENTED_EDGE('',*,*,#6790,.T.);
#8519=ORIENTED_EDGE('',*,*,#6792,.F.);
#8520=ORIENTED_EDGE('',*,*,#6782,.F.);
#8521=ORIENTED_EDGE('',*,*,#6792,.T.);
#8522=ORIENTED_EDGE('',*,*,#6789,.T.);
#8523=ORIENTED_EDGE('',*,*,#6786,.T.);
#8524=ORIENTED_EDGE('',*,*,#6783,.T.);
#8525=ORIENTED_EDGE('',*,*,#6791,.F.);
#8526=ORIENTED_EDGE('',*,*,#6781,.F.);
#8527=ORIENTED_EDGE('',*,*,#6785,.F.);
#8528=ORIENTED_EDGE('',*,*,#6788,.F.);
#8529=ORIENTED_EDGE('',*,*,#6793,.F.);
#8530=ORIENTED_EDGE('',*,*,#6794,.T.);
#8531=ORIENTED_EDGE('',*,*,#6795,.F.);
#8532=ORIENTED_EDGE('',*,*,#6794,.F.);
#8533=ORIENTED_EDGE('',*,*,#6793,.T.);
#8534=ORIENTED_EDGE('',*,*,#6796,.F.);
#8535=ORIENTED_EDGE('',*,*,#6797,.T.);
#8536=ORIENTED_EDGE('',*,*,#6798,.F.);
#8537=ORIENTED_EDGE('',*,*,#6797,.F.);
#8538=ORIENTED_EDGE('',*,*,#6796,.T.);
#8539=ORIENTED_EDGE('',*,*,#6799,.F.);
#8540=ORIENTED_EDGE('',*,*,#6800,.F.);
#8541=ORIENTED_EDGE('',*,*,#6801,.F.);
#8542=ORIENTED_EDGE('',*,*,#6802,.F.);
#8543=ORIENTED_EDGE('',*,*,#6803,.F.);
#8544=ORIENTED_EDGE('',*,*,#6804,.F.);
#8545=ORIENTED_EDGE('',*,*,#6805,.F.);
#8546=ORIENTED_EDGE('',*,*,#6806,.F.);
#8547=ORIENTED_EDGE('',*,*,#6800,.T.);
#8548=ORIENTED_EDGE('',*,*,#6807,.F.);
#8549=ORIENTED_EDGE('',*,*,#6808,.F.);
#8550=ORIENTED_EDGE('',*,*,#6809,.F.);
#8551=ORIENTED_EDGE('',*,*,#6810,.F.);
#8552=ORIENTED_EDGE('',*,*,#6811,.F.);
#8553=ORIENTED_EDGE('',*,*,#6806,.T.);
#8554=ORIENTED_EDGE('',*,*,#6812,.T.);
#8555=ORIENTED_EDGE('',*,*,#6801,.T.);
#8556=ORIENTED_EDGE('',*,*,#6812,.F.);
#8557=ORIENTED_EDGE('',*,*,#6805,.T.);
#8558=ORIENTED_EDGE('',*,*,#6813,.F.);
#8559=ORIENTED_EDGE('',*,*,#6803,.T.);
#8560=ORIENTED_EDGE('',*,*,#6811,.T.);
#8561=ORIENTED_EDGE('',*,*,#6814,.T.);
#8562=ORIENTED_EDGE('',*,*,#6815,.F.);
#8563=ORIENTED_EDGE('',*,*,#6799,.T.);
#8564=ORIENTED_EDGE('',*,*,#6816,.F.);
#8565=ORIENTED_EDGE('',*,*,#6817,.F.);
#8566=ORIENTED_EDGE('',*,*,#6807,.T.);
#8567=ORIENTED_EDGE('',*,*,#6802,.T.);
#8568=ORIENTED_EDGE('',*,*,#6813,.T.);
#8569=ORIENTED_EDGE('',*,*,#6804,.T.);
#8570=ORIENTED_EDGE('',*,*,#6815,.T.);
#8571=ORIENTED_EDGE('',*,*,#6818,.T.);
#8572=ORIENTED_EDGE('',*,*,#6819,.F.);
#8573=ORIENTED_EDGE('',*,*,#6820,.T.);
#8574=ORIENTED_EDGE('',*,*,#6816,.T.);
#8575=ORIENTED_EDGE('',*,*,#6795,.T.);
#8576=ORIENTED_EDGE('',*,*,#6798,.T.);
#8577=ORIENTED_EDGE('',*,*,#6821,.F.);
#8578=ORIENTED_EDGE('',*,*,#6818,.F.);
#8579=ORIENTED_EDGE('',*,*,#6814,.F.);
#8580=ORIENTED_EDGE('',*,*,#6810,.T.);
#8581=ORIENTED_EDGE('',*,*,#6822,.F.);
#8582=ORIENTED_EDGE('',*,*,#6808,.T.);
#8583=ORIENTED_EDGE('',*,*,#6817,.T.);
#8584=ORIENTED_EDGE('',*,*,#6820,.F.);
#8585=ORIENTED_EDGE('',*,*,#6823,.F.);
#8586=ORIENTED_EDGE('',*,*,#6824,.T.);
#8587=ORIENTED_EDGE('',*,*,#6825,.F.);
#8588=ORIENTED_EDGE('',*,*,#6824,.F.);
#8589=ORIENTED_EDGE('',*,*,#6823,.T.);
#8590=ORIENTED_EDGE('',*,*,#6826,.F.);
#8591=ORIENTED_EDGE('',*,*,#6827,.T.);
#8592=ORIENTED_EDGE('',*,*,#6828,.F.);
#8593=ORIENTED_EDGE('',*,*,#6827,.F.);
#8594=ORIENTED_EDGE('',*,*,#6826,.T.);
#8595=ORIENTED_EDGE('',*,*,#6829,.F.);
#8596=ORIENTED_EDGE('',*,*,#6830,.F.);
#8597=ORIENTED_EDGE('',*,*,#6831,.F.);
#8598=ORIENTED_EDGE('',*,*,#6832,.F.);
#8599=ORIENTED_EDGE('',*,*,#6833,.F.);
#8600=ORIENTED_EDGE('',*,*,#6834,.F.);
#8601=ORIENTED_EDGE('',*,*,#6835,.F.);
#8602=ORIENTED_EDGE('',*,*,#6836,.F.);
#8603=ORIENTED_EDGE('',*,*,#6830,.T.);
#8604=ORIENTED_EDGE('',*,*,#6837,.F.);
#8605=ORIENTED_EDGE('',*,*,#6838,.F.);
#8606=ORIENTED_EDGE('',*,*,#6839,.F.);
#8607=ORIENTED_EDGE('',*,*,#6840,.F.);
#8608=ORIENTED_EDGE('',*,*,#6841,.F.);
#8609=ORIENTED_EDGE('',*,*,#6842,.T.);
#8610=ORIENTED_EDGE('',*,*,#6843,.T.);
#8611=ORIENTED_EDGE('',*,*,#6844,.F.);
#8612=ORIENTED_EDGE('',*,*,#6845,.F.);
#8613=ORIENTED_EDGE('',*,*,#6846,.F.);
#8614=ORIENTED_EDGE('',*,*,#6847,.F.);
#8615=ORIENTED_EDGE('',*,*,#6848,.F.);
#8616=ORIENTED_EDGE('',*,*,#6836,.T.);
#8617=ORIENTED_EDGE('',*,*,#6849,.T.);
#8618=ORIENTED_EDGE('',*,*,#6831,.T.);
#8619=ORIENTED_EDGE('',*,*,#6849,.F.);
#8620=ORIENTED_EDGE('',*,*,#6835,.T.);
#8621=ORIENTED_EDGE('',*,*,#6850,.F.);
#8622=ORIENTED_EDGE('',*,*,#6833,.T.);
#8623=ORIENTED_EDGE('',*,*,#6848,.T.);
#8624=ORIENTED_EDGE('',*,*,#6851,.T.);
#8625=ORIENTED_EDGE('',*,*,#6852,.F.);
#8626=ORIENTED_EDGE('',*,*,#6829,.T.);
#8627=ORIENTED_EDGE('',*,*,#6853,.F.);
#8628=ORIENTED_EDGE('',*,*,#6854,.F.);
#8629=ORIENTED_EDGE('',*,*,#6837,.T.);
#8630=ORIENTED_EDGE('',*,*,#6832,.T.);
#8631=ORIENTED_EDGE('',*,*,#6850,.T.);
#8632=ORIENTED_EDGE('',*,*,#6834,.T.);
#8633=ORIENTED_EDGE('',*,*,#6852,.T.);
#8634=ORIENTED_EDGE('',*,*,#6855,.T.);
#8635=ORIENTED_EDGE('',*,*,#6856,.F.);
#8636=ORIENTED_EDGE('',*,*,#6857,.T.);
#8637=ORIENTED_EDGE('',*,*,#6853,.T.);
#8638=ORIENTED_EDGE('',*,*,#6825,.T.);
#8639=ORIENTED_EDGE('',*,*,#6828,.T.);
#8640=ORIENTED_EDGE('',*,*,#6858,.F.);
#8641=ORIENTED_EDGE('',*,*,#6838,.T.);
#8642=ORIENTED_EDGE('',*,*,#6854,.T.);
#8643=ORIENTED_EDGE('',*,*,#6857,.F.);
#8644=ORIENTED_EDGE('',*,*,#6859,.F.);
#8645=ORIENTED_EDGE('',*,*,#6855,.F.);
#8646=ORIENTED_EDGE('',*,*,#6851,.F.);
#8647=ORIENTED_EDGE('',*,*,#6847,.T.);
#8648=ORIENTED_EDGE('',*,*,#6858,.T.);
#8649=ORIENTED_EDGE('',*,*,#6856,.T.);
#8650=ORIENTED_EDGE('',*,*,#6859,.T.);
#8651=ORIENTED_EDGE('',*,*,#6846,.T.);
#8652=ORIENTED_EDGE('',*,*,#6860,.T.);
#8653=ORIENTED_EDGE('',*,*,#6861,.F.);
#8654=ORIENTED_EDGE('',*,*,#6862,.F.);
#8655=ORIENTED_EDGE('',*,*,#6839,.T.);
#8656=ORIENTED_EDGE('',*,*,#6821,.T.);
#8657=ORIENTED_EDGE('',*,*,#6809,.T.);
#8658=ORIENTED_EDGE('',*,*,#6822,.T.);
#8659=ORIENTED_EDGE('',*,*,#6819,.T.);
#8660=ORIENTED_EDGE('',*,*,#6863,.F.);
#8661=ORIENTED_EDGE('',*,*,#6864,.T.);
#8662=ORIENTED_EDGE('',*,*,#6865,.F.);
#8663=ORIENTED_EDGE('',*,*,#6866,.F.);
#8664=ORIENTED_EDGE('',*,*,#6867,.F.);
#8665=ORIENTED_EDGE('',*,*,#6868,.T.);
#8666=ORIENTED_EDGE('',*,*,#6869,.F.);
#8667=ORIENTED_EDGE('',*,*,#6870,.F.);
#8668=ORIENTED_EDGE('',*,*,#6868,.F.);
#8669=ORIENTED_EDGE('',*,*,#6871,.F.);
#8670=ORIENTED_EDGE('',*,*,#6864,.F.);
#8671=ORIENTED_EDGE('',*,*,#6872,.F.);
#8672=ORIENTED_EDGE('',*,*,#6866,.T.);
#8673=ORIENTED_EDGE('',*,*,#6873,.F.);
#8674=ORIENTED_EDGE('',*,*,#6874,.T.);
#8675=ORIENTED_EDGE('',*,*,#6875,.F.);
#8676=ORIENTED_EDGE('',*,*,#6876,.T.);
#8677=ORIENTED_EDGE('',*,*,#6877,.T.);
#8678=ORIENTED_EDGE('',*,*,#6876,.F.);
#8679=ORIENTED_EDGE('',*,*,#6871,.T.);
#8680=ORIENTED_EDGE('',*,*,#6867,.T.);
#8681=ORIENTED_EDGE('',*,*,#6872,.T.);
#8682=ORIENTED_EDGE('',*,*,#6865,.T.);
#8683=ORIENTED_EDGE('',*,*,#6863,.T.);
#8684=ORIENTED_EDGE('',*,*,#6842,.F.);
#8685=ORIENTED_EDGE('',*,*,#6874,.F.);
#8686=ORIENTED_EDGE('',*,*,#6843,.F.);
#8687=ORIENTED_EDGE('',*,*,#6878,.T.);
#8688=ORIENTED_EDGE('',*,*,#6879,.T.);
#8689=ORIENTED_EDGE('',*,*,#6878,.F.);
#8690=ORIENTED_EDGE('',*,*,#6869,.T.);
#8691=ORIENTED_EDGE('',*,*,#6870,.T.);
#8692=ORIENTED_EDGE('',*,*,#6879,.F.);
#8693=ORIENTED_EDGE('',*,*,#6877,.F.);
#8694=ORIENTED_EDGE('',*,*,#6840,.T.);
#8695=ORIENTED_EDGE('',*,*,#6862,.T.);
#8696=ORIENTED_EDGE('',*,*,#6880,.F.);
#8697=ORIENTED_EDGE('',*,*,#6881,.F.);
#8698=ORIENTED_EDGE('',*,*,#6841,.T.);
#8699=ORIENTED_EDGE('',*,*,#6881,.T.);
#8700=ORIENTED_EDGE('',*,*,#6882,.F.);
#8701=ORIENTED_EDGE('',*,*,#6883,.F.);
#8702=ORIENTED_EDGE('',*,*,#6844,.T.);
#8703=ORIENTED_EDGE('',*,*,#6873,.T.);
#8704=ORIENTED_EDGE('',*,*,#6845,.T.);
#8705=ORIENTED_EDGE('',*,*,#6883,.T.);
#8706=ORIENTED_EDGE('',*,*,#6884,.F.);
#8707=ORIENTED_EDGE('',*,*,#6860,.F.);
#8708=ORIENTED_EDGE('',*,*,#6861,.T.);
#8709=ORIENTED_EDGE('',*,*,#6884,.T.);
#8710=ORIENTED_EDGE('',*,*,#6882,.T.);
#8711=ORIENTED_EDGE('',*,*,#6880,.T.);
#8712=ORIENTED_EDGE('',*,*,#6875,.T.);
#8713=ORIENTED_EDGE('',*,*,#6885,.F.);
#8714=ORIENTED_EDGE('',*,*,#6886,.T.);
#8715=ORIENTED_EDGE('',*,*,#6887,.F.);
#8716=ORIENTED_EDGE('',*,*,#6888,.F.);
#8717=ORIENTED_EDGE('',*,*,#6889,.F.);
#8718=ORIENTED_EDGE('',*,*,#6886,.F.);
#8719=ORIENTED_EDGE('',*,*,#6890,.F.);
#8720=ORIENTED_EDGE('',*,*,#6891,.T.);
#8721=ORIENTED_EDGE('',*,*,#6892,.F.);
#8722=ORIENTED_EDGE('',*,*,#6893,.F.);
#8723=ORIENTED_EDGE('',*,*,#6894,.F.);
#8724=ORIENTED_EDGE('',*,*,#6891,.F.);
#8725=ORIENTED_EDGE('',*,*,#6895,.T.);
#8726=ORIENTED_EDGE('',*,*,#6896,.T.);
#8727=ORIENTED_EDGE('',*,*,#6897,.T.);
#8728=ORIENTED_EDGE('',*,*,#6893,.T.);
#8729=ORIENTED_EDGE('',*,*,#6898,.T.);
#8730=ORIENTED_EDGE('',*,*,#6888,.T.);
#8731=ORIENTED_EDGE('',*,*,#6899,.F.);
#8732=ORIENTED_EDGE('',*,*,#6900,.F.);
#8733=ORIENTED_EDGE('',*,*,#6901,.F.);
#8734=ORIENTED_EDGE('',*,*,#6902,.T.);
#8735=ORIENTED_EDGE('',*,*,#6903,.F.);
#8736=ORIENTED_EDGE('',*,*,#6904,.F.);
#8737=ORIENTED_EDGE('',*,*,#6905,.F.);
#8738=ORIENTED_EDGE('',*,*,#6906,.T.);
#8739=ORIENTED_EDGE('',*,*,#6907,.F.);
#8740=ORIENTED_EDGE('',*,*,#6908,.F.);
#8741=ORIENTED_EDGE('',*,*,#6906,.F.);
#8742=ORIENTED_EDGE('',*,*,#6909,.F.);
#8743=ORIENTED_EDGE('',*,*,#6902,.F.);
#8744=ORIENTED_EDGE('',*,*,#6910,.F.);
#8745=ORIENTED_EDGE('',*,*,#6904,.T.);
#8746=ORIENTED_EDGE('',*,*,#6911,.F.);
#8747=ORIENTED_EDGE('',*,*,#6912,.T.);
#8748=ORIENTED_EDGE('',*,*,#6899,.T.);
#8749=ORIENTED_EDGE('',*,*,#6912,.F.);
#8750=ORIENTED_EDGE('',*,*,#6913,.F.);
#8751=ORIENTED_EDGE('',*,*,#6914,.T.);
#8752=ORIENTED_EDGE('',*,*,#6900,.T.);
#8753=ORIENTED_EDGE('',*,*,#6914,.F.);
#8754=ORIENTED_EDGE('',*,*,#6915,.F.);
#8755=ORIENTED_EDGE('',*,*,#6916,.T.);
#8756=ORIENTED_EDGE('',*,*,#6896,.F.);
#8757=ORIENTED_EDGE('',*,*,#6887,.T.);
#8758=ORIENTED_EDGE('',*,*,#6889,.T.);
#8759=ORIENTED_EDGE('',*,*,#6885,.T.);
#8760=ORIENTED_EDGE('',*,*,#6898,.F.);
#8761=ORIENTED_EDGE('',*,*,#6892,.T.);
#8762=ORIENTED_EDGE('',*,*,#6894,.T.);
#8763=ORIENTED_EDGE('',*,*,#6890,.T.);
#8764=ORIENTED_EDGE('',*,*,#6897,.F.);
#8765=ORIENTED_EDGE('',*,*,#6916,.F.);
#8766=ORIENTED_EDGE('',*,*,#6907,.T.);
#8767=ORIENTED_EDGE('',*,*,#6908,.T.);
#8768=ORIENTED_EDGE('',*,*,#6915,.T.);
#8769=ORIENTED_EDGE('',*,*,#6917,.T.);
#8770=ORIENTED_EDGE('',*,*,#6917,.F.);
#8771=ORIENTED_EDGE('',*,*,#6918,.T.);
#8772=ORIENTED_EDGE('',*,*,#6919,.T.);
#8773=ORIENTED_EDGE('',*,*,#6918,.F.);
#8774=ORIENTED_EDGE('',*,*,#6909,.T.);
#8775=ORIENTED_EDGE('',*,*,#6905,.T.);
#8776=ORIENTED_EDGE('',*,*,#6910,.T.);
#8777=ORIENTED_EDGE('',*,*,#6903,.T.);
#8778=ORIENTED_EDGE('',*,*,#6901,.T.);
#8779=ORIENTED_EDGE('',*,*,#6895,.F.);
#8780=ORIENTED_EDGE('',*,*,#6920,.T.);
#8781=ORIENTED_EDGE('',*,*,#6921,.T.);
#8782=ORIENTED_EDGE('',*,*,#6920,.F.);
#8783=ORIENTED_EDGE('',*,*,#6921,.F.);
#8784=ORIENTED_EDGE('',*,*,#6911,.T.);
#8785=ORIENTED_EDGE('',*,*,#6913,.T.);
#8786=ORIENTED_EDGE('',*,*,#6919,.F.);
#8787=ORIENTED_EDGE('',*,*,#6922,.F.);
#8788=ORIENTED_EDGE('',*,*,#6923,.T.);
#8789=ORIENTED_EDGE('',*,*,#6924,.F.);
#8790=ORIENTED_EDGE('',*,*,#6925,.F.);
#8791=ORIENTED_EDGE('',*,*,#6926,.F.);
#8792=ORIENTED_EDGE('',*,*,#6927,.F.);
#8793=ORIENTED_EDGE('',*,*,#6928,.F.);
#8794=ORIENTED_EDGE('',*,*,#6929,.F.);
#8795=ORIENTED_EDGE('',*,*,#6930,.F.);
#8796=ORIENTED_EDGE('',*,*,#6931,.F.);
#8797=ORIENTED_EDGE('',*,*,#6932,.F.);
#8798=ORIENTED_EDGE('',*,*,#6933,.F.);
#8799=ORIENTED_EDGE('',*,*,#6934,.F.);
#8800=ORIENTED_EDGE('',*,*,#6927,.T.);
#8801=ORIENTED_EDGE('',*,*,#6935,.F.);
#8802=ORIENTED_EDGE('',*,*,#6936,.F.);
#8803=ORIENTED_EDGE('',*,*,#6937,.F.);
#8804=ORIENTED_EDGE('',*,*,#6938,.F.);
#8805=ORIENTED_EDGE('',*,*,#6939,.F.);
#8806=ORIENTED_EDGE('',*,*,#6923,.F.);
#8807=ORIENTED_EDGE('',*,*,#6928,.T.);
#8808=ORIENTED_EDGE('',*,*,#6934,.T.);
#8809=ORIENTED_EDGE('',*,*,#6940,.F.);
#8810=ORIENTED_EDGE('',*,*,#6935,.T.);
#8811=ORIENTED_EDGE('',*,*,#6922,.T.);
#8812=ORIENTED_EDGE('',*,*,#6941,.F.);
#8813=ORIENTED_EDGE('',*,*,#6929,.T.);
#8814=ORIENTED_EDGE('',*,*,#6941,.T.);
#8815=ORIENTED_EDGE('',*,*,#6925,.T.);
#8816=ORIENTED_EDGE('',*,*,#6942,.F.);
#8817=ORIENTED_EDGE('',*,*,#6933,.T.);
#8818=ORIENTED_EDGE('',*,*,#6943,.F.);
#8819=ORIENTED_EDGE('',*,*,#6936,.T.);
#8820=ORIENTED_EDGE('',*,*,#6940,.T.);
#8821=ORIENTED_EDGE('',*,*,#6932,.T.);
#8822=ORIENTED_EDGE('',*,*,#6944,.F.);
#8823=ORIENTED_EDGE('',*,*,#6937,.T.);
#8824=ORIENTED_EDGE('',*,*,#6943,.T.);
#8825=ORIENTED_EDGE('',*,*,#6931,.T.);
#8826=ORIENTED_EDGE('',*,*,#6945,.F.);
#8827=ORIENTED_EDGE('',*,*,#6938,.T.);
#8828=ORIENTED_EDGE('',*,*,#6944,.T.);
#8829=ORIENTED_EDGE('',*,*,#6926,.T.);
#8830=ORIENTED_EDGE('',*,*,#6942,.T.);
#8831=ORIENTED_EDGE('',*,*,#6924,.T.);
#8832=ORIENTED_EDGE('',*,*,#6939,.T.);
#8833=ORIENTED_EDGE('',*,*,#6945,.T.);
#8834=ORIENTED_EDGE('',*,*,#6930,.T.);
#8835=ORIENTED_EDGE('',*,*,#6946,.F.);
#8836=ORIENTED_EDGE('',*,*,#6947,.T.);
#8837=ORIENTED_EDGE('',*,*,#6948,.F.);
#8838=ORIENTED_EDGE('',*,*,#6947,.F.);
#8839=ORIENTED_EDGE('',*,*,#6949,.F.);
#8840=ORIENTED_EDGE('',*,*,#6950,.T.);
#8841=ORIENTED_EDGE('',*,*,#6951,.F.);
#8842=ORIENTED_EDGE('',*,*,#6950,.F.);
#8843=ORIENTED_EDGE('',*,*,#6952,.F.);
#8844=ORIENTED_EDGE('',*,*,#6953,.T.);
#8845=ORIENTED_EDGE('',*,*,#6954,.F.);
#8846=ORIENTED_EDGE('',*,*,#6955,.F.);
#8847=ORIENTED_EDGE('',*,*,#6956,.F.);
#8848=ORIENTED_EDGE('',*,*,#6957,.F.);
#8849=ORIENTED_EDGE('',*,*,#6958,.F.);
#8850=ORIENTED_EDGE('',*,*,#6959,.F.);
#8851=ORIENTED_EDGE('',*,*,#6960,.F.);
#8852=ORIENTED_EDGE('',*,*,#6961,.F.);
#8853=ORIENTED_EDGE('',*,*,#6962,.F.);
#8854=ORIENTED_EDGE('',*,*,#6957,.T.);
#8855=ORIENTED_EDGE('',*,*,#6963,.F.);
#8856=ORIENTED_EDGE('',*,*,#6964,.F.);
#8857=ORIENTED_EDGE('',*,*,#6965,.F.);
#8858=ORIENTED_EDGE('',*,*,#6953,.F.);
#8859=ORIENTED_EDGE('',*,*,#6955,.T.);
#8860=ORIENTED_EDGE('',*,*,#6966,.F.);
#8861=ORIENTED_EDGE('',*,*,#6967,.F.);
#8862=ORIENTED_EDGE('',*,*,#6968,.T.);
#8863=ORIENTED_EDGE('',*,*,#6959,.T.);
#8864=ORIENTED_EDGE('',*,*,#6969,.T.);
#8865=ORIENTED_EDGE('',*,*,#6970,.T.);
#8866=ORIENTED_EDGE('',*,*,#6971,.F.);
#8867=ORIENTED_EDGE('',*,*,#6954,.T.);
#8868=ORIENTED_EDGE('',*,*,#6965,.T.);
#8869=ORIENTED_EDGE('',*,*,#6972,.T.);
#8870=ORIENTED_EDGE('',*,*,#6960,.T.);
#8871=ORIENTED_EDGE('',*,*,#6956,.T.);
#8872=ORIENTED_EDGE('',*,*,#6971,.T.);
#8873=ORIENTED_EDGE('',*,*,#6973,.T.);
#8874=ORIENTED_EDGE('',*,*,#6974,.T.);
#8875=ORIENTED_EDGE('',*,*,#6975,.T.);
#8876=ORIENTED_EDGE('',*,*,#6966,.T.);
#8877=ORIENTED_EDGE('',*,*,#6948,.T.);
#8878=ORIENTED_EDGE('',*,*,#6951,.T.);
#8879=ORIENTED_EDGE('',*,*,#6964,.T.);
#8880=ORIENTED_EDGE('',*,*,#6976,.F.);
#8881=ORIENTED_EDGE('',*,*,#6961,.T.);
#8882=ORIENTED_EDGE('',*,*,#6972,.F.);
#8883=ORIENTED_EDGE('',*,*,#6977,.T.);
#8884=ORIENTED_EDGE('',*,*,#6967,.T.);
#8885=ORIENTED_EDGE('',*,*,#6975,.F.);
#8886=ORIENTED_EDGE('',*,*,#6978,.F.);
#8887=ORIENTED_EDGE('',*,*,#6979,.T.);
#8888=ORIENTED_EDGE('',*,*,#6978,.T.);
#8889=ORIENTED_EDGE('',*,*,#6974,.F.);
#8890=ORIENTED_EDGE('',*,*,#6980,.F.);
#8891=ORIENTED_EDGE('',*,*,#6981,.T.);
#8892=ORIENTED_EDGE('',*,*,#6980,.T.);
#8893=ORIENTED_EDGE('',*,*,#6973,.F.);
#8894=ORIENTED_EDGE('',*,*,#6970,.F.);
#8895=ORIENTED_EDGE('',*,*,#6952,.T.);
#8896=ORIENTED_EDGE('',*,*,#6968,.F.);
#8897=ORIENTED_EDGE('',*,*,#6977,.F.);
#8898=ORIENTED_EDGE('',*,*,#6979,.F.);
#8899=ORIENTED_EDGE('',*,*,#6981,.F.);
#8900=ORIENTED_EDGE('',*,*,#6969,.F.);
#8901=ORIENTED_EDGE('',*,*,#6958,.T.);
#8902=ORIENTED_EDGE('',*,*,#6962,.T.);
#8903=ORIENTED_EDGE('',*,*,#6976,.T.);
#8904=ORIENTED_EDGE('',*,*,#6963,.T.);
#8905=ORIENTED_EDGE('',*,*,#6946,.T.);
#8906=ORIENTED_EDGE('',*,*,#6949,.T.);
#8907=ORIENTED_EDGE('',*,*,#6982,.F.);
#8908=ORIENTED_EDGE('',*,*,#6983,.T.);
#8909=ORIENTED_EDGE('',*,*,#6984,.F.);
#8910=ORIENTED_EDGE('',*,*,#6985,.F.);
#8911=ORIENTED_EDGE('',*,*,#6986,.F.);
#8912=ORIENTED_EDGE('',*,*,#6987,.F.);
#8913=ORIENTED_EDGE('',*,*,#6988,.F.);
#8914=ORIENTED_EDGE('',*,*,#6989,.F.);
#8915=ORIENTED_EDGE('',*,*,#6990,.F.);
#8916=ORIENTED_EDGE('',*,*,#6991,.F.);
#8917=ORIENTED_EDGE('',*,*,#6992,.F.);
#8918=ORIENTED_EDGE('',*,*,#6993,.F.);
#8919=ORIENTED_EDGE('',*,*,#6994,.F.);
#8920=ORIENTED_EDGE('',*,*,#6987,.T.);
#8921=ORIENTED_EDGE('',*,*,#6995,.F.);
#8922=ORIENTED_EDGE('',*,*,#6996,.F.);
#8923=ORIENTED_EDGE('',*,*,#6997,.F.);
#8924=ORIENTED_EDGE('',*,*,#6998,.F.);
#8925=ORIENTED_EDGE('',*,*,#6999,.F.);
#8926=ORIENTED_EDGE('',*,*,#6983,.F.);
#8927=ORIENTED_EDGE('',*,*,#6988,.T.);
#8928=ORIENTED_EDGE('',*,*,#6994,.T.);
#8929=ORIENTED_EDGE('',*,*,#7000,.F.);
#8930=ORIENTED_EDGE('',*,*,#6995,.T.);
#8931=ORIENTED_EDGE('',*,*,#6982,.T.);
#8932=ORIENTED_EDGE('',*,*,#7001,.F.);
#8933=ORIENTED_EDGE('',*,*,#6989,.T.);
#8934=ORIENTED_EDGE('',*,*,#7001,.T.);
#8935=ORIENTED_EDGE('',*,*,#6985,.T.);
#8936=ORIENTED_EDGE('',*,*,#7002,.F.);
#8937=ORIENTED_EDGE('',*,*,#6993,.T.);
#8938=ORIENTED_EDGE('',*,*,#7003,.F.);
#8939=ORIENTED_EDGE('',*,*,#6996,.T.);
#8940=ORIENTED_EDGE('',*,*,#7000,.T.);
#8941=ORIENTED_EDGE('',*,*,#6992,.T.);
#8942=ORIENTED_EDGE('',*,*,#7004,.F.);
#8943=ORIENTED_EDGE('',*,*,#6997,.T.);
#8944=ORIENTED_EDGE('',*,*,#7003,.T.);
#8945=ORIENTED_EDGE('',*,*,#6991,.T.);
#8946=ORIENTED_EDGE('',*,*,#7005,.F.);
#8947=ORIENTED_EDGE('',*,*,#6998,.T.);
#8948=ORIENTED_EDGE('',*,*,#7004,.T.);
#8949=ORIENTED_EDGE('',*,*,#6986,.T.);
#8950=ORIENTED_EDGE('',*,*,#7002,.T.);
#8951=ORIENTED_EDGE('',*,*,#6984,.T.);
#8952=ORIENTED_EDGE('',*,*,#6999,.T.);
#8953=ORIENTED_EDGE('',*,*,#7005,.T.);
#8954=ORIENTED_EDGE('',*,*,#6990,.T.);
#8955=ORIENTED_EDGE('',*,*,#7006,.F.);
#8956=ORIENTED_EDGE('',*,*,#7007,.T.);
#8957=ORIENTED_EDGE('',*,*,#7008,.F.);
#8958=ORIENTED_EDGE('',*,*,#7007,.F.);
#8959=ORIENTED_EDGE('',*,*,#7009,.F.);
#8960=ORIENTED_EDGE('',*,*,#7010,.T.);
#8961=ORIENTED_EDGE('',*,*,#7011,.F.);
#8962=ORIENTED_EDGE('',*,*,#7010,.F.);
#8963=ORIENTED_EDGE('',*,*,#7012,.F.);
#8964=ORIENTED_EDGE('',*,*,#7013,.T.);
#8965=ORIENTED_EDGE('',*,*,#7014,.F.);
#8966=ORIENTED_EDGE('',*,*,#7015,.F.);
#8967=ORIENTED_EDGE('',*,*,#7016,.F.);
#8968=ORIENTED_EDGE('',*,*,#7017,.F.);
#8969=ORIENTED_EDGE('',*,*,#7018,.F.);
#8970=ORIENTED_EDGE('',*,*,#7019,.F.);
#8971=ORIENTED_EDGE('',*,*,#7020,.F.);
#8972=ORIENTED_EDGE('',*,*,#7021,.F.);
#8973=ORIENTED_EDGE('',*,*,#7022,.F.);
#8974=ORIENTED_EDGE('',*,*,#7017,.T.);
#8975=ORIENTED_EDGE('',*,*,#7023,.F.);
#8976=ORIENTED_EDGE('',*,*,#7024,.F.);
#8977=ORIENTED_EDGE('',*,*,#7025,.F.);
#8978=ORIENTED_EDGE('',*,*,#7013,.F.);
#8979=ORIENTED_EDGE('',*,*,#7015,.T.);
#8980=ORIENTED_EDGE('',*,*,#7026,.F.);
#8981=ORIENTED_EDGE('',*,*,#7027,.F.);
#8982=ORIENTED_EDGE('',*,*,#7028,.T.);
#8983=ORIENTED_EDGE('',*,*,#7019,.T.);
#8984=ORIENTED_EDGE('',*,*,#7029,.T.);
#8985=ORIENTED_EDGE('',*,*,#7030,.T.);
#8986=ORIENTED_EDGE('',*,*,#7031,.F.);
#8987=ORIENTED_EDGE('',*,*,#7014,.T.);
#8988=ORIENTED_EDGE('',*,*,#7025,.T.);
#8989=ORIENTED_EDGE('',*,*,#7032,.T.);
#8990=ORIENTED_EDGE('',*,*,#7020,.T.);
#8991=ORIENTED_EDGE('',*,*,#7016,.T.);
#8992=ORIENTED_EDGE('',*,*,#7031,.T.);
#8993=ORIENTED_EDGE('',*,*,#7033,.T.);
#8994=ORIENTED_EDGE('',*,*,#7034,.T.);
#8995=ORIENTED_EDGE('',*,*,#7035,.T.);
#8996=ORIENTED_EDGE('',*,*,#7026,.T.);
#8997=ORIENTED_EDGE('',*,*,#7008,.T.);
#8998=ORIENTED_EDGE('',*,*,#7011,.T.);
#8999=ORIENTED_EDGE('',*,*,#7024,.T.);
#9000=ORIENTED_EDGE('',*,*,#7036,.F.);
#9001=ORIENTED_EDGE('',*,*,#7021,.T.);
#9002=ORIENTED_EDGE('',*,*,#7032,.F.);
#9003=ORIENTED_EDGE('',*,*,#7037,.T.);
#9004=ORIENTED_EDGE('',*,*,#7027,.T.);
#9005=ORIENTED_EDGE('',*,*,#7035,.F.);
#9006=ORIENTED_EDGE('',*,*,#7038,.F.);
#9007=ORIENTED_EDGE('',*,*,#7039,.T.);
#9008=ORIENTED_EDGE('',*,*,#7038,.T.);
#9009=ORIENTED_EDGE('',*,*,#7034,.F.);
#9010=ORIENTED_EDGE('',*,*,#7040,.F.);
#9011=ORIENTED_EDGE('',*,*,#7041,.T.);
#9012=ORIENTED_EDGE('',*,*,#7040,.T.);
#9013=ORIENTED_EDGE('',*,*,#7033,.F.);
#9014=ORIENTED_EDGE('',*,*,#7030,.F.);
#9015=ORIENTED_EDGE('',*,*,#7012,.T.);
#9016=ORIENTED_EDGE('',*,*,#7028,.F.);
#9017=ORIENTED_EDGE('',*,*,#7037,.F.);
#9018=ORIENTED_EDGE('',*,*,#7039,.F.);
#9019=ORIENTED_EDGE('',*,*,#7041,.F.);
#9020=ORIENTED_EDGE('',*,*,#7029,.F.);
#9021=ORIENTED_EDGE('',*,*,#7018,.T.);
#9022=ORIENTED_EDGE('',*,*,#7022,.T.);
#9023=ORIENTED_EDGE('',*,*,#7036,.T.);
#9024=ORIENTED_EDGE('',*,*,#7023,.T.);
#9025=ORIENTED_EDGE('',*,*,#7006,.T.);
#9026=ORIENTED_EDGE('',*,*,#7009,.T.);
#9027=ORIENTED_EDGE('',*,*,#7042,.F.);
#9028=ORIENTED_EDGE('',*,*,#7043,.F.);
#9029=ORIENTED_EDGE('',*,*,#7044,.F.);
#9030=ORIENTED_EDGE('',*,*,#7045,.F.);
#9031=ORIENTED_EDGE('',*,*,#7045,.T.);
#9032=ORIENTED_EDGE('',*,*,#7046,.F.);
#9033=ORIENTED_EDGE('',*,*,#7047,.T.);
#9034=ORIENTED_EDGE('',*,*,#7048,.F.);
#9035=ORIENTED_EDGE('',*,*,#7044,.T.);
#9036=ORIENTED_EDGE('',*,*,#7049,.F.);
#9037=ORIENTED_EDGE('',*,*,#7050,.T.);
#9038=ORIENTED_EDGE('',*,*,#7046,.T.);
#9039=ORIENTED_EDGE('',*,*,#7051,.T.);
#9040=ORIENTED_EDGE('',*,*,#7052,.T.);
#9041=ORIENTED_EDGE('',*,*,#7053,.F.);
#9042=ORIENTED_EDGE('',*,*,#7047,.F.);
#9043=ORIENTED_EDGE('',*,*,#7050,.F.);
#9044=ORIENTED_EDGE('',*,*,#7054,.F.);
#9045=ORIENTED_EDGE('',*,*,#7043,.T.);
#9046=ORIENTED_EDGE('',*,*,#7055,.F.);
#9047=ORIENTED_EDGE('',*,*,#7054,.T.);
#9048=ORIENTED_EDGE('',*,*,#7049,.T.);
#9049=ORIENTED_EDGE('',*,*,#7042,.T.);
#9050=ORIENTED_EDGE('',*,*,#7048,.T.);
#9051=ORIENTED_EDGE('',*,*,#7053,.T.);
#9052=ORIENTED_EDGE('',*,*,#7055,.T.);
#9053=ORIENTED_EDGE('',*,*,#7056,.T.);
#9054=ORIENTED_EDGE('',*,*,#7057,.T.);
#9055=ORIENTED_EDGE('',*,*,#7058,.F.);
#9056=ORIENTED_EDGE('',*,*,#7059,.T.);
#9057=ORIENTED_EDGE('',*,*,#7060,.F.);
#9058=ORIENTED_EDGE('',*,*,#7061,.F.);
#9059=ORIENTED_EDGE('',*,*,#7062,.F.);
#9060=ORIENTED_EDGE('',*,*,#7063,.T.);
#9061=ORIENTED_EDGE('',*,*,#7064,.F.);
#9062=ORIENTED_EDGE('',*,*,#7065,.F.);
#9063=ORIENTED_EDGE('',*,*,#7063,.F.);
#9064=ORIENTED_EDGE('',*,*,#7066,.F.);
#9065=ORIENTED_EDGE('',*,*,#7059,.F.);
#9066=ORIENTED_EDGE('',*,*,#7067,.F.);
#9067=ORIENTED_EDGE('',*,*,#7061,.T.);
#9068=ORIENTED_EDGE('',*,*,#7051,.F.);
#9069=ORIENTED_EDGE('',*,*,#7068,.T.);
#9070=ORIENTED_EDGE('',*,*,#7057,.F.);
#9071=ORIENTED_EDGE('',*,*,#7068,.F.);
#9072=ORIENTED_EDGE('',*,*,#7069,.F.);
#9073=ORIENTED_EDGE('',*,*,#7070,.T.);
#9074=ORIENTED_EDGE('',*,*,#7056,.F.);
#9075=ORIENTED_EDGE('',*,*,#7070,.F.);
#9076=ORIENTED_EDGE('',*,*,#7066,.T.);
#9077=ORIENTED_EDGE('',*,*,#7062,.T.);
#9078=ORIENTED_EDGE('',*,*,#7067,.T.);
#9079=ORIENTED_EDGE('',*,*,#7060,.T.);
#9080=ORIENTED_EDGE('',*,*,#7058,.T.);
#9081=ORIENTED_EDGE('',*,*,#7052,.F.);
#9082=ORIENTED_EDGE('',*,*,#7071,.T.);
#9083=ORIENTED_EDGE('',*,*,#7072,.T.);
#9084=ORIENTED_EDGE('',*,*,#7071,.F.);
#9085=ORIENTED_EDGE('',*,*,#7064,.T.);
#9086=ORIENTED_EDGE('',*,*,#7065,.T.);
#9087=ORIENTED_EDGE('',*,*,#7072,.F.);
#9088=ORIENTED_EDGE('',*,*,#7069,.T.);
#9089=ORIENTED_EDGE('',*,*,#7073,.F.);
#9090=ORIENTED_EDGE('',*,*,#7074,.T.);
#9091=ORIENTED_EDGE('',*,*,#7075,.F.);
#9092=ORIENTED_EDGE('',*,*,#7074,.F.);
#9093=ORIENTED_EDGE('',*,*,#7076,.F.);
#9094=ORIENTED_EDGE('',*,*,#7077,.T.);
#9095=ORIENTED_EDGE('',*,*,#7078,.F.);
#9096=ORIENTED_EDGE('',*,*,#7077,.F.);
#9097=ORIENTED_EDGE('',*,*,#7079,.F.);
#9098=ORIENTED_EDGE('',*,*,#7080,.T.);
#9099=ORIENTED_EDGE('',*,*,#7081,.F.);
#9100=ORIENTED_EDGE('',*,*,#7080,.F.);
#9101=ORIENTED_EDGE('',*,*,#7082,.F.);
#9102=ORIENTED_EDGE('',*,*,#7083,.T.);
#9103=ORIENTED_EDGE('',*,*,#7084,.F.);
#9104=ORIENTED_EDGE('',*,*,#7083,.F.);
#9105=ORIENTED_EDGE('',*,*,#7085,.F.);
#9106=ORIENTED_EDGE('',*,*,#7086,.T.);
#9107=ORIENTED_EDGE('',*,*,#7087,.F.);
#9108=ORIENTED_EDGE('',*,*,#7086,.F.);
#9109=ORIENTED_EDGE('',*,*,#7088,.F.);
#9110=ORIENTED_EDGE('',*,*,#7089,.T.);
#9111=ORIENTED_EDGE('',*,*,#7090,.F.);
#9112=ORIENTED_EDGE('',*,*,#7089,.F.);
#9113=ORIENTED_EDGE('',*,*,#7091,.F.);
#9114=ORIENTED_EDGE('',*,*,#7092,.T.);
#9115=ORIENTED_EDGE('',*,*,#7093,.F.);
#9116=ORIENTED_EDGE('',*,*,#7092,.F.);
#9117=ORIENTED_EDGE('',*,*,#7094,.F.);
#9118=ORIENTED_EDGE('',*,*,#7095,.F.);
#9119=ORIENTED_EDGE('',*,*,#7096,.T.);
#9120=ORIENTED_EDGE('',*,*,#7097,.F.);
#9121=ORIENTED_EDGE('',*,*,#7090,.T.);
#9122=ORIENTED_EDGE('',*,*,#7098,.F.);
#9123=ORIENTED_EDGE('',*,*,#7099,.F.);
#9124=ORIENTED_EDGE('',*,*,#7100,.F.);
#9125=ORIENTED_EDGE('',*,*,#7101,.F.);
#9126=ORIENTED_EDGE('',*,*,#7087,.T.);
#9127=ORIENTED_EDGE('',*,*,#7102,.F.);
#9128=ORIENTED_EDGE('',*,*,#7100,.T.);
#9129=ORIENTED_EDGE('',*,*,#7103,.F.);
#9130=ORIENTED_EDGE('',*,*,#7104,.F.);
#9131=ORIENTED_EDGE('',*,*,#7105,.F.);
#9132=ORIENTED_EDGE('',*,*,#7106,.T.);
#9133=ORIENTED_EDGE('',*,*,#7107,.F.);
#9134=ORIENTED_EDGE('',*,*,#7096,.F.);
#9135=ORIENTED_EDGE('',*,*,#7108,.T.);
#9136=ORIENTED_EDGE('',*,*,#7109,.F.);
#9137=ORIENTED_EDGE('',*,*,#7110,.F.);
#9138=ORIENTED_EDGE('',*,*,#7101,.T.);
#9139=ORIENTED_EDGE('',*,*,#7102,.T.);
#9140=ORIENTED_EDGE('',*,*,#7111,.T.);
#9141=ORIENTED_EDGE('',*,*,#7105,.T.);
#9142=ORIENTED_EDGE('',*,*,#7095,.T.);
#9143=ORIENTED_EDGE('',*,*,#7091,.T.);
#9144=ORIENTED_EDGE('',*,*,#7082,.T.);
#9145=ORIENTED_EDGE('',*,*,#7079,.T.);
#9146=ORIENTED_EDGE('',*,*,#7076,.T.);
#9147=ORIENTED_EDGE('',*,*,#7073,.T.);
#9148=ORIENTED_EDGE('',*,*,#7094,.T.);
#9149=ORIENTED_EDGE('',*,*,#7112,.T.);
#9150=ORIENTED_EDGE('',*,*,#7113,.F.);
#9151=ORIENTED_EDGE('',*,*,#7108,.F.);
#9152=ORIENTED_EDGE('',*,*,#7114,.T.);
#9153=ORIENTED_EDGE('',*,*,#7115,.F.);
#9154=ORIENTED_EDGE('',*,*,#7112,.F.);
#9155=ORIENTED_EDGE('',*,*,#7097,.T.);
#9156=ORIENTED_EDGE('',*,*,#7107,.T.);
#9157=ORIENTED_EDGE('',*,*,#7116,.T.);
#9158=ORIENTED_EDGE('',*,*,#7103,.T.);
#9159=ORIENTED_EDGE('',*,*,#7099,.T.);
#9160=ORIENTED_EDGE('',*,*,#7093,.T.);
#9161=ORIENTED_EDGE('',*,*,#7084,.T.);
#9162=ORIENTED_EDGE('',*,*,#7081,.T.);
#9163=ORIENTED_EDGE('',*,*,#7078,.T.);
#9164=ORIENTED_EDGE('',*,*,#7075,.T.);
#9165=ORIENTED_EDGE('',*,*,#7098,.T.);
#9166=ORIENTED_EDGE('',*,*,#7110,.T.);
#9167=ORIENTED_EDGE('',*,*,#7117,.F.);
#9168=ORIENTED_EDGE('',*,*,#7114,.F.);
#9169=ORIENTED_EDGE('',*,*,#7117,.T.);
#9170=ORIENTED_EDGE('',*,*,#7109,.T.);
#9171=ORIENTED_EDGE('',*,*,#7113,.T.);
#9172=ORIENTED_EDGE('',*,*,#7115,.T.);
#9173=ORIENTED_EDGE('',*,*,#7116,.F.);
#9174=ORIENTED_EDGE('',*,*,#7106,.F.);
#9175=ORIENTED_EDGE('',*,*,#7111,.F.);
#9176=ORIENTED_EDGE('',*,*,#7104,.T.);
#9177=ORIENTED_EDGE('',*,*,#7085,.T.);
#9178=ORIENTED_EDGE('',*,*,#7088,.T.);
#9179=ORIENTED_EDGE('',*,*,#7118,.F.);
#9180=ORIENTED_EDGE('',*,*,#7119,.T.);
#9181=ORIENTED_EDGE('',*,*,#7120,.F.);
#9182=ORIENTED_EDGE('',*,*,#7119,.F.);
#9183=ORIENTED_EDGE('',*,*,#7121,.F.);
#9184=ORIENTED_EDGE('',*,*,#7122,.T.);
#9185=ORIENTED_EDGE('',*,*,#7123,.F.);
#9186=ORIENTED_EDGE('',*,*,#7122,.F.);
#9187=ORIENTED_EDGE('',*,*,#7124,.F.);
#9188=ORIENTED_EDGE('',*,*,#7125,.T.);
#9189=ORIENTED_EDGE('',*,*,#7126,.F.);
#9190=ORIENTED_EDGE('',*,*,#7125,.F.);
#9191=ORIENTED_EDGE('',*,*,#7127,.F.);
#9192=ORIENTED_EDGE('',*,*,#7128,.T.);
#9193=ORIENTED_EDGE('',*,*,#7129,.F.);
#9194=ORIENTED_EDGE('',*,*,#7128,.F.);
#9195=ORIENTED_EDGE('',*,*,#7130,.F.);
#9196=ORIENTED_EDGE('',*,*,#7131,.T.);
#9197=ORIENTED_EDGE('',*,*,#7132,.F.);
#9198=ORIENTED_EDGE('',*,*,#7131,.F.);
#9199=ORIENTED_EDGE('',*,*,#7130,.T.);
#9200=ORIENTED_EDGE('',*,*,#7133,.T.);
#9201=ORIENTED_EDGE('',*,*,#7133,.F.);
#9202=ORIENTED_EDGE('',*,*,#7134,.T.);
#9203=ORIENTED_EDGE('',*,*,#7135,.T.);
#9204=ORIENTED_EDGE('',*,*,#7134,.F.);
#9205=ORIENTED_EDGE('',*,*,#7136,.F.);
#9206=ORIENTED_EDGE('',*,*,#7137,.T.);
#9207=ORIENTED_EDGE('',*,*,#7138,.T.);
#9208=ORIENTED_EDGE('',*,*,#7137,.F.);
#9209=ORIENTED_EDGE('',*,*,#7136,.T.);
#9210=ORIENTED_EDGE('',*,*,#7132,.T.);
#9211=ORIENTED_EDGE('',*,*,#7129,.T.);
#9212=ORIENTED_EDGE('',*,*,#7126,.T.);
#9213=ORIENTED_EDGE('',*,*,#7123,.T.);
#9214=ORIENTED_EDGE('',*,*,#7120,.T.);
#9215=ORIENTED_EDGE('',*,*,#7138,.F.);
#9216=ORIENTED_EDGE('',*,*,#7135,.F.);
#9217=ORIENTED_EDGE('',*,*,#7127,.T.);
#9218=ORIENTED_EDGE('',*,*,#7124,.T.);
#9219=ORIENTED_EDGE('',*,*,#7121,.T.);
#9220=ORIENTED_EDGE('',*,*,#7118,.T.);
#9221=ORIENTED_EDGE('',*,*,#7139,.F.);
#9222=ORIENTED_EDGE('',*,*,#7140,.T.);
#9223=ORIENTED_EDGE('',*,*,#7141,.F.);
#9224=ORIENTED_EDGE('',*,*,#7140,.F.);
#9225=ORIENTED_EDGE('',*,*,#7142,.F.);
#9226=ORIENTED_EDGE('',*,*,#7143,.T.);
#9227=ORIENTED_EDGE('',*,*,#7144,.F.);
#9228=ORIENTED_EDGE('',*,*,#7143,.F.);
#9229=ORIENTED_EDGE('',*,*,#7145,.F.);
#9230=ORIENTED_EDGE('',*,*,#7146,.T.);
#9231=ORIENTED_EDGE('',*,*,#7147,.F.);
#9232=ORIENTED_EDGE('',*,*,#7146,.F.);
#9233=ORIENTED_EDGE('',*,*,#7148,.F.);
#9234=ORIENTED_EDGE('',*,*,#7149,.T.);
#9235=ORIENTED_EDGE('',*,*,#7150,.F.);
#9236=ORIENTED_EDGE('',*,*,#7149,.F.);
#9237=ORIENTED_EDGE('',*,*,#7151,.F.);
#9238=ORIENTED_EDGE('',*,*,#7152,.T.);
#9239=ORIENTED_EDGE('',*,*,#7153,.T.);
#9240=ORIENTED_EDGE('',*,*,#7152,.F.);
#9241=ORIENTED_EDGE('',*,*,#7153,.F.);
#9242=ORIENTED_EDGE('',*,*,#7154,.F.);
#9243=ORIENTED_EDGE('',*,*,#7155,.F.);
#9244=ORIENTED_EDGE('',*,*,#7156,.T.);
#9245=ORIENTED_EDGE('',*,*,#7154,.T.);
#9246=ORIENTED_EDGE('',*,*,#7156,.F.);
#9247=ORIENTED_EDGE('',*,*,#7157,.F.);
#9248=ORIENTED_EDGE('',*,*,#7158,.T.);
#9249=ORIENTED_EDGE('',*,*,#7159,.T.);
#9250=ORIENTED_EDGE('',*,*,#7158,.F.);
#9251=ORIENTED_EDGE('',*,*,#7157,.T.);
#9252=ORIENTED_EDGE('',*,*,#7155,.T.);
#9253=ORIENTED_EDGE('',*,*,#7150,.T.);
#9254=ORIENTED_EDGE('',*,*,#7147,.T.);
#9255=ORIENTED_EDGE('',*,*,#7144,.T.);
#9256=ORIENTED_EDGE('',*,*,#7141,.T.);
#9257=ORIENTED_EDGE('',*,*,#7159,.F.);
#9258=ORIENTED_EDGE('',*,*,#7151,.T.);
#9259=ORIENTED_EDGE('',*,*,#7148,.T.);
#9260=ORIENTED_EDGE('',*,*,#7145,.T.);
#9261=ORIENTED_EDGE('',*,*,#7142,.T.);
#9262=ORIENTED_EDGE('',*,*,#7139,.T.);
#9263=ORIENTED_EDGE('',*,*,#7160,.F.);
#9264=ORIENTED_EDGE('',*,*,#7161,.T.);
#9265=ORIENTED_EDGE('',*,*,#7162,.F.);
#9266=ORIENTED_EDGE('',*,*,#7161,.F.);
#9267=ORIENTED_EDGE('',*,*,#7163,.F.);
#9268=ORIENTED_EDGE('',*,*,#7164,.T.);
#9269=ORIENTED_EDGE('',*,*,#7165,.F.);
#9270=ORIENTED_EDGE('',*,*,#7164,.F.);
#9271=ORIENTED_EDGE('',*,*,#7166,.F.);
#9272=ORIENTED_EDGE('',*,*,#7167,.T.);
#9273=ORIENTED_EDGE('',*,*,#7168,.F.);
#9274=ORIENTED_EDGE('',*,*,#7167,.F.);
#9275=ORIENTED_EDGE('',*,*,#7169,.F.);
#9276=ORIENTED_EDGE('',*,*,#7170,.T.);
#9277=ORIENTED_EDGE('',*,*,#7171,.F.);
#9278=ORIENTED_EDGE('',*,*,#7170,.F.);
#9279=ORIENTED_EDGE('',*,*,#7172,.F.);
#9280=ORIENTED_EDGE('',*,*,#7173,.T.);
#9281=ORIENTED_EDGE('',*,*,#7174,.F.);
#9282=ORIENTED_EDGE('',*,*,#7173,.F.);
#9283=ORIENTED_EDGE('',*,*,#7175,.F.);
#9284=ORIENTED_EDGE('',*,*,#7176,.T.);
#9285=ORIENTED_EDGE('',*,*,#7177,.F.);
#9286=ORIENTED_EDGE('',*,*,#7176,.F.);
#9287=ORIENTED_EDGE('',*,*,#7178,.F.);
#9288=ORIENTED_EDGE('',*,*,#7179,.T.);
#9289=ORIENTED_EDGE('',*,*,#7180,.F.);
#9290=ORIENTED_EDGE('',*,*,#7179,.F.);
#9291=ORIENTED_EDGE('',*,*,#7181,.F.);
#9292=ORIENTED_EDGE('',*,*,#7182,.F.);
#9293=ORIENTED_EDGE('',*,*,#7183,.T.);
#9294=ORIENTED_EDGE('',*,*,#7184,.F.);
#9295=ORIENTED_EDGE('',*,*,#7177,.T.);
#9296=ORIENTED_EDGE('',*,*,#7185,.F.);
#9297=ORIENTED_EDGE('',*,*,#7186,.F.);
#9298=ORIENTED_EDGE('',*,*,#7187,.F.);
#9299=ORIENTED_EDGE('',*,*,#7188,.F.);
#9300=ORIENTED_EDGE('',*,*,#7174,.T.);
#9301=ORIENTED_EDGE('',*,*,#7189,.F.);
#9302=ORIENTED_EDGE('',*,*,#7187,.T.);
#9303=ORIENTED_EDGE('',*,*,#7190,.F.);
#9304=ORIENTED_EDGE('',*,*,#7191,.F.);
#9305=ORIENTED_EDGE('',*,*,#7192,.F.);
#9306=ORIENTED_EDGE('',*,*,#7193,.T.);
#9307=ORIENTED_EDGE('',*,*,#7194,.F.);
#9308=ORIENTED_EDGE('',*,*,#7183,.F.);
#9309=ORIENTED_EDGE('',*,*,#7195,.T.);
#9310=ORIENTED_EDGE('',*,*,#7196,.F.);
#9311=ORIENTED_EDGE('',*,*,#7197,.F.);
#9312=ORIENTED_EDGE('',*,*,#7188,.T.);
#9313=ORIENTED_EDGE('',*,*,#7189,.T.);
#9314=ORIENTED_EDGE('',*,*,#7198,.T.);
#9315=ORIENTED_EDGE('',*,*,#7192,.T.);
#9316=ORIENTED_EDGE('',*,*,#7182,.T.);
#9317=ORIENTED_EDGE('',*,*,#7178,.T.);
#9318=ORIENTED_EDGE('',*,*,#7169,.T.);
#9319=ORIENTED_EDGE('',*,*,#7166,.T.);
#9320=ORIENTED_EDGE('',*,*,#7163,.T.);
#9321=ORIENTED_EDGE('',*,*,#7160,.T.);
#9322=ORIENTED_EDGE('',*,*,#7181,.T.);
#9323=ORIENTED_EDGE('',*,*,#7199,.T.);
#9324=ORIENTED_EDGE('',*,*,#7200,.F.);
#9325=ORIENTED_EDGE('',*,*,#7195,.F.);
#9326=ORIENTED_EDGE('',*,*,#7201,.T.);
#9327=ORIENTED_EDGE('',*,*,#7202,.F.);
#9328=ORIENTED_EDGE('',*,*,#7199,.F.);
#9329=ORIENTED_EDGE('',*,*,#7184,.T.);
#9330=ORIENTED_EDGE('',*,*,#7194,.T.);
#9331=ORIENTED_EDGE('',*,*,#7203,.T.);
#9332=ORIENTED_EDGE('',*,*,#7190,.T.);
#9333=ORIENTED_EDGE('',*,*,#7186,.T.);
#9334=ORIENTED_EDGE('',*,*,#7180,.T.);
#9335=ORIENTED_EDGE('',*,*,#7171,.T.);
#9336=ORIENTED_EDGE('',*,*,#7168,.T.);
#9337=ORIENTED_EDGE('',*,*,#7165,.T.);
#9338=ORIENTED_EDGE('',*,*,#7162,.T.);
#9339=ORIENTED_EDGE('',*,*,#7185,.T.);
#9340=ORIENTED_EDGE('',*,*,#7197,.T.);
#9341=ORIENTED_EDGE('',*,*,#7204,.F.);
#9342=ORIENTED_EDGE('',*,*,#7201,.F.);
#9343=ORIENTED_EDGE('',*,*,#7204,.T.);
#9344=ORIENTED_EDGE('',*,*,#7196,.T.);
#9345=ORIENTED_EDGE('',*,*,#7200,.T.);
#9346=ORIENTED_EDGE('',*,*,#7202,.T.);
#9347=ORIENTED_EDGE('',*,*,#7203,.F.);
#9348=ORIENTED_EDGE('',*,*,#7193,.F.);
#9349=ORIENTED_EDGE('',*,*,#7198,.F.);
#9350=ORIENTED_EDGE('',*,*,#7191,.T.);
#9351=ORIENTED_EDGE('',*,*,#7172,.T.);
#9352=ORIENTED_EDGE('',*,*,#7175,.T.);
#9353=ORIENTED_EDGE('',*,*,#7205,.F.);
#9354=ORIENTED_EDGE('',*,*,#7206,.T.);
#9355=ORIENTED_EDGE('',*,*,#7207,.F.);
#9356=ORIENTED_EDGE('',*,*,#7206,.F.);
#9357=ORIENTED_EDGE('',*,*,#7208,.F.);
#9358=ORIENTED_EDGE('',*,*,#7209,.T.);
#9359=ORIENTED_EDGE('',*,*,#7210,.F.);
#9360=ORIENTED_EDGE('',*,*,#7209,.F.);
#9361=ORIENTED_EDGE('',*,*,#7211,.F.);
#9362=ORIENTED_EDGE('',*,*,#7212,.T.);
#9363=ORIENTED_EDGE('',*,*,#7213,.F.);
#9364=ORIENTED_EDGE('',*,*,#7212,.F.);
#9365=ORIENTED_EDGE('',*,*,#7214,.F.);
#9366=ORIENTED_EDGE('',*,*,#7215,.T.);
#9367=ORIENTED_EDGE('',*,*,#7216,.F.);
#9368=ORIENTED_EDGE('',*,*,#7215,.F.);
#9369=ORIENTED_EDGE('',*,*,#7217,.F.);
#9370=ORIENTED_EDGE('',*,*,#7218,.T.);
#9371=ORIENTED_EDGE('',*,*,#7219,.F.);
#9372=ORIENTED_EDGE('',*,*,#7218,.F.);
#9373=ORIENTED_EDGE('',*,*,#7217,.T.);
#9374=ORIENTED_EDGE('',*,*,#7220,.T.);
#9375=ORIENTED_EDGE('',*,*,#7220,.F.);
#9376=ORIENTED_EDGE('',*,*,#7221,.T.);
#9377=ORIENTED_EDGE('',*,*,#7222,.T.);
#9378=ORIENTED_EDGE('',*,*,#7221,.F.);
#9379=ORIENTED_EDGE('',*,*,#7223,.F.);
#9380=ORIENTED_EDGE('',*,*,#7224,.T.);
#9381=ORIENTED_EDGE('',*,*,#7225,.T.);
#9382=ORIENTED_EDGE('',*,*,#7224,.F.);
#9383=ORIENTED_EDGE('',*,*,#7223,.T.);
#9384=ORIENTED_EDGE('',*,*,#7219,.T.);
#9385=ORIENTED_EDGE('',*,*,#7216,.T.);
#9386=ORIENTED_EDGE('',*,*,#7213,.T.);
#9387=ORIENTED_EDGE('',*,*,#7210,.T.);
#9388=ORIENTED_EDGE('',*,*,#7207,.T.);
#9389=ORIENTED_EDGE('',*,*,#7225,.F.);
#9390=ORIENTED_EDGE('',*,*,#7222,.F.);
#9391=ORIENTED_EDGE('',*,*,#7214,.T.);
#9392=ORIENTED_EDGE('',*,*,#7211,.T.);
#9393=ORIENTED_EDGE('',*,*,#7208,.T.);
#9394=ORIENTED_EDGE('',*,*,#7205,.T.);
#9395=ORIENTED_EDGE('',*,*,#7226,.F.);
#9396=ORIENTED_EDGE('',*,*,#7227,.T.);
#9397=ORIENTED_EDGE('',*,*,#7228,.F.);
#9398=ORIENTED_EDGE('',*,*,#7227,.F.);
#9399=ORIENTED_EDGE('',*,*,#7229,.F.);
#9400=ORIENTED_EDGE('',*,*,#7230,.T.);
#9401=ORIENTED_EDGE('',*,*,#7231,.F.);
#9402=ORIENTED_EDGE('',*,*,#7230,.F.);
#9403=ORIENTED_EDGE('',*,*,#7232,.F.);
#9404=ORIENTED_EDGE('',*,*,#7233,.T.);
#9405=ORIENTED_EDGE('',*,*,#7234,.F.);
#9406=ORIENTED_EDGE('',*,*,#7233,.F.);
#9407=ORIENTED_EDGE('',*,*,#7235,.F.);
#9408=ORIENTED_EDGE('',*,*,#7236,.T.);
#9409=ORIENTED_EDGE('',*,*,#7237,.F.);
#9410=ORIENTED_EDGE('',*,*,#7236,.F.);
#9411=ORIENTED_EDGE('',*,*,#7238,.F.);
#9412=ORIENTED_EDGE('',*,*,#7239,.T.);
#9413=ORIENTED_EDGE('',*,*,#7240,.T.);
#9414=ORIENTED_EDGE('',*,*,#7239,.F.);
#9415=ORIENTED_EDGE('',*,*,#7240,.F.);
#9416=ORIENTED_EDGE('',*,*,#7241,.F.);
#9417=ORIENTED_EDGE('',*,*,#7242,.F.);
#9418=ORIENTED_EDGE('',*,*,#7243,.T.);
#9419=ORIENTED_EDGE('',*,*,#7241,.T.);
#9420=ORIENTED_EDGE('',*,*,#7243,.F.);
#9421=ORIENTED_EDGE('',*,*,#7244,.F.);
#9422=ORIENTED_EDGE('',*,*,#7245,.T.);
#9423=ORIENTED_EDGE('',*,*,#7246,.T.);
#9424=ORIENTED_EDGE('',*,*,#7245,.F.);
#9425=ORIENTED_EDGE('',*,*,#7244,.T.);
#9426=ORIENTED_EDGE('',*,*,#7242,.T.);
#9427=ORIENTED_EDGE('',*,*,#7237,.T.);
#9428=ORIENTED_EDGE('',*,*,#7234,.T.);
#9429=ORIENTED_EDGE('',*,*,#7231,.T.);
#9430=ORIENTED_EDGE('',*,*,#7228,.T.);
#9431=ORIENTED_EDGE('',*,*,#7246,.F.);
#9432=ORIENTED_EDGE('',*,*,#7238,.T.);
#9433=ORIENTED_EDGE('',*,*,#7235,.T.);
#9434=ORIENTED_EDGE('',*,*,#7232,.T.);
#9435=ORIENTED_EDGE('',*,*,#7229,.T.);
#9436=ORIENTED_EDGE('',*,*,#7226,.T.);
#9437=ORIENTED_EDGE('',*,*,#7247,.F.);
#9438=ORIENTED_EDGE('',*,*,#7248,.T.);
#9439=ORIENTED_EDGE('',*,*,#7249,.T.);
#9440=ORIENTED_EDGE('',*,*,#7250,.T.);
#9441=ORIENTED_EDGE('',*,*,#7249,.F.);
#9442=ORIENTED_EDGE('',*,*,#7247,.T.);
#9443=ORIENTED_EDGE('',*,*,#7251,.T.);
#9444=ORIENTED_EDGE('',*,*,#7248,.F.);
#9445=ORIENTED_EDGE('',*,*,#7251,.F.);
#9446=ORIENTED_EDGE('',*,*,#7250,.F.);
#9447=ORIENTED_EDGE('',*,*,#7252,.F.);
#9448=ORIENTED_EDGE('',*,*,#7253,.F.);
#9449=ORIENTED_EDGE('',*,*,#7254,.T.);
#9450=ORIENTED_EDGE('',*,*,#7255,.F.);
#9451=ORIENTED_EDGE('',*,*,#7256,.F.);
#9452=ORIENTED_EDGE('',*,*,#7254,.F.);
#9453=ORIENTED_EDGE('',*,*,#7255,.T.);
#9454=ORIENTED_EDGE('',*,*,#7256,.T.);
#9455=ORIENTED_EDGE('',*,*,#7257,.T.);
#9456=ORIENTED_EDGE('',*,*,#7258,.T.);
#9457=ORIENTED_EDGE('',*,*,#7257,.F.);
#9458=ORIENTED_EDGE('',*,*,#7259,.T.);
#9459=ORIENTED_EDGE('',*,*,#7260,.T.);
#9460=ORIENTED_EDGE('',*,*,#7261,.F.);
#9461=ORIENTED_EDGE('',*,*,#7260,.F.);
#9462=ORIENTED_EDGE('',*,*,#7261,.T.);
#9463=ORIENTED_EDGE('',*,*,#7262,.T.);
#9464=ORIENTED_EDGE('',*,*,#7263,.F.);
#9465=ORIENTED_EDGE('',*,*,#7262,.F.);
#9466=ORIENTED_EDGE('',*,*,#7258,.F.);
#9467=ORIENTED_EDGE('',*,*,#7263,.T.);
#9468=ORIENTED_EDGE('',*,*,#7264,.F.);
#9469=ORIENTED_EDGE('',*,*,#7265,.T.);
#9470=ORIENTED_EDGE('',*,*,#7252,.T.);
#9471=ORIENTED_EDGE('',*,*,#7253,.T.);
#9472=ORIENTED_EDGE('',*,*,#7265,.F.);
#9473=ORIENTED_EDGE('',*,*,#7264,.T.);
#9474=ORIENTED_EDGE('',*,*,#7266,.F.);
#9475=ORIENTED_EDGE('',*,*,#7266,.T.);
#9476=ORIENTED_EDGE('',*,*,#7267,.T.);
#9477=ORIENTED_EDGE('',*,*,#7259,.F.);
#9478=ORIENTED_EDGE('',*,*,#7267,.F.);
#9479=ORIENTED_EDGE('',*,*,#7268,.F.);
#9480=ORIENTED_EDGE('',*,*,#7269,.F.);
#9481=ORIENTED_EDGE('',*,*,#7270,.T.);
#9482=ORIENTED_EDGE('',*,*,#7271,.F.);
#9483=ORIENTED_EDGE('',*,*,#7272,.F.);
#9484=ORIENTED_EDGE('',*,*,#7270,.F.);
#9485=ORIENTED_EDGE('',*,*,#7273,.T.);
#9486=ORIENTED_EDGE('',*,*,#7274,.T.);
#9487=ORIENTED_EDGE('',*,*,#7271,.T.);
#9488=ORIENTED_EDGE('',*,*,#7272,.T.);
#9489=ORIENTED_EDGE('',*,*,#7274,.F.);
#9490=ORIENTED_EDGE('',*,*,#7275,.F.);
#9491=ORIENTED_EDGE('',*,*,#7276,.T.);
#9492=ORIENTED_EDGE('',*,*,#7277,.F.);
#9493=ORIENTED_EDGE('',*,*,#7278,.T.);
#9494=ORIENTED_EDGE('',*,*,#7275,.T.);
#9495=ORIENTED_EDGE('',*,*,#7278,.F.);
#9496=ORIENTED_EDGE('',*,*,#7279,.F.);
#9497=ORIENTED_EDGE('',*,*,#7280,.T.);
#9498=ORIENTED_EDGE('',*,*,#7277,.T.);
#9499=ORIENTED_EDGE('',*,*,#7280,.F.);
#9500=ORIENTED_EDGE('',*,*,#7281,.F.);
#9501=ORIENTED_EDGE('',*,*,#7282,.T.);
#9502=ORIENTED_EDGE('',*,*,#7279,.T.);
#9503=ORIENTED_EDGE('',*,*,#7282,.F.);
#9504=ORIENTED_EDGE('',*,*,#7281,.T.);
#9505=ORIENTED_EDGE('',*,*,#7273,.F.);
#9506=ORIENTED_EDGE('',*,*,#7268,.T.);
#9507=ORIENTED_EDGE('',*,*,#7269,.T.);
#9508=ORIENTED_EDGE('',*,*,#7283,.T.);
#9509=ORIENTED_EDGE('',*,*,#7276,.F.);
#9510=ORIENTED_EDGE('',*,*,#7283,.F.);
#9511=ORIENTED_EDGE('',*,*,#7284,.T.);
#9512=ORIENTED_EDGE('',*,*,#7284,.F.);
#9513=ORIENTED_EDGE('',*,*,#7285,.T.);
#9514=ORIENTED_EDGE('',*,*,#7285,.F.);
#9515=ORIENTED_EDGE('',*,*,#7286,.T.);
#9516=ORIENTED_EDGE('',*,*,#7286,.F.);
#9517=ORIENTED_EDGE('',*,*,#7287,.T.);
#9518=ORIENTED_EDGE('',*,*,#7287,.F.);
#9519=ORIENTED_EDGE('',*,*,#7288,.T.);
#9520=ORIENTED_EDGE('',*,*,#7288,.F.);
#9521=ORIENTED_EDGE('',*,*,#7289,.T.);
#9522=ORIENTED_EDGE('',*,*,#7289,.F.);
#9523=ORIENTED_EDGE('',*,*,#7290,.T.);
#9524=ORIENTED_EDGE('',*,*,#7290,.F.);
#9525=ORIENTED_EDGE('',*,*,#7291,.F.);
#9526=ORIENTED_EDGE('',*,*,#7292,.F.);
#9527=ORIENTED_EDGE('',*,*,#7293,.F.);
#9528=ORIENTED_EDGE('',*,*,#7294,.F.);
#9529=ORIENTED_EDGE('',*,*,#7293,.T.);
#9530=ORIENTED_EDGE('',*,*,#7295,.F.);
#9531=ORIENTED_EDGE('',*,*,#7296,.T.);
#9532=ORIENTED_EDGE('',*,*,#7297,.F.);
#9533=ORIENTED_EDGE('',*,*,#7298,.T.);
#9534=ORIENTED_EDGE('',*,*,#7299,.F.);
#9535=ORIENTED_EDGE('',*,*,#7300,.T.);
#9536=ORIENTED_EDGE('',*,*,#7301,.F.);
#9537=ORIENTED_EDGE('',*,*,#7300,.F.);
#9538=ORIENTED_EDGE('',*,*,#7302,.F.);
#9539=ORIENTED_EDGE('',*,*,#7303,.T.);
#9540=ORIENTED_EDGE('',*,*,#7304,.F.);
#9541=ORIENTED_EDGE('',*,*,#7305,.T.);
#9542=ORIENTED_EDGE('',*,*,#7306,.F.);
#9543=ORIENTED_EDGE('',*,*,#7307,.T.);
#9544=ORIENTED_EDGE('',*,*,#7308,.F.);
#9545=ORIENTED_EDGE('',*,*,#7309,.T.);
#9546=ORIENTED_EDGE('',*,*,#7310,.F.);
#9547=ORIENTED_EDGE('',*,*,#7292,.T.);
#9548=ORIENTED_EDGE('',*,*,#7311,.T.);
#9549=ORIENTED_EDGE('',*,*,#7312,.T.);
#9550=ORIENTED_EDGE('',*,*,#7295,.T.);
#9551=ORIENTED_EDGE('',*,*,#7313,.F.);
#9552=ORIENTED_EDGE('',*,*,#7314,.F.);
#9553=ORIENTED_EDGE('',*,*,#7296,.F.);
#9554=ORIENTED_EDGE('',*,*,#7312,.F.);
#9555=ORIENTED_EDGE('',*,*,#7314,.T.);
#9556=ORIENTED_EDGE('',*,*,#7315,.T.);
#9557=ORIENTED_EDGE('',*,*,#7316,.T.);
#9558=ORIENTED_EDGE('',*,*,#7297,.T.);
#9559=ORIENTED_EDGE('',*,*,#7317,.F.);
#9560=ORIENTED_EDGE('',*,*,#7318,.F.);
#9561=ORIENTED_EDGE('',*,*,#7298,.F.);
#9562=ORIENTED_EDGE('',*,*,#7316,.F.);
#9563=ORIENTED_EDGE('',*,*,#7318,.T.);
#9564=ORIENTED_EDGE('',*,*,#7319,.T.);
#9565=ORIENTED_EDGE('',*,*,#7320,.T.);
#9566=ORIENTED_EDGE('',*,*,#7321,.T.);
#9567=ORIENTED_EDGE('',*,*,#7302,.T.);
#9568=ORIENTED_EDGE('',*,*,#7299,.T.);
#9569=ORIENTED_EDGE('',*,*,#7322,.F.);
#9570=ORIENTED_EDGE('',*,*,#7323,.F.);
#9571=ORIENTED_EDGE('',*,*,#7303,.F.);
#9572=ORIENTED_EDGE('',*,*,#7321,.F.);
#9573=ORIENTED_EDGE('',*,*,#7323,.T.);
#9574=ORIENTED_EDGE('',*,*,#7324,.T.);
#9575=ORIENTED_EDGE('',*,*,#7325,.T.);
#9576=ORIENTED_EDGE('',*,*,#7304,.T.);
#9577=ORIENTED_EDGE('',*,*,#7326,.F.);
#9578=ORIENTED_EDGE('',*,*,#7327,.F.);
#9579=ORIENTED_EDGE('',*,*,#7305,.F.);
#9580=ORIENTED_EDGE('',*,*,#7325,.F.);
#9581=ORIENTED_EDGE('',*,*,#7327,.T.);
#9582=ORIENTED_EDGE('',*,*,#7328,.T.);
#9583=ORIENTED_EDGE('',*,*,#7329,.T.);
#9584=ORIENTED_EDGE('',*,*,#7306,.T.);
#9585=ORIENTED_EDGE('',*,*,#7307,.F.);
#9586=ORIENTED_EDGE('',*,*,#7329,.F.);
#9587=ORIENTED_EDGE('',*,*,#7330,.F.);
#9588=ORIENTED_EDGE('',*,*,#7331,.F.);
#9589=ORIENTED_EDGE('',*,*,#7332,.F.);
#9590=ORIENTED_EDGE('',*,*,#7333,.T.);
#9591=ORIENTED_EDGE('',*,*,#7319,.F.);
#9592=ORIENTED_EDGE('',*,*,#7317,.T.);
#9593=ORIENTED_EDGE('',*,*,#7315,.F.);
#9594=ORIENTED_EDGE('',*,*,#7313,.T.);
#9595=ORIENTED_EDGE('',*,*,#7311,.F.);
#9596=ORIENTED_EDGE('',*,*,#7291,.T.);
#9597=ORIENTED_EDGE('',*,*,#7334,.F.);
#9598=ORIENTED_EDGE('',*,*,#7335,.T.);
#9599=ORIENTED_EDGE('',*,*,#7336,.F.);
#9600=ORIENTED_EDGE('',*,*,#7330,.T.);
#9601=ORIENTED_EDGE('',*,*,#7328,.F.);
#9602=ORIENTED_EDGE('',*,*,#7326,.T.);
#9603=ORIENTED_EDGE('',*,*,#7324,.F.);
#9604=ORIENTED_EDGE('',*,*,#7322,.T.);
#9605=ORIENTED_EDGE('',*,*,#7320,.F.);
#9606=ORIENTED_EDGE('',*,*,#7333,.F.);
#9607=ORIENTED_EDGE('',*,*,#7294,.T.);
#9608=ORIENTED_EDGE('',*,*,#7310,.T.);
#9609=ORIENTED_EDGE('',*,*,#7337,.T.);
#9610=ORIENTED_EDGE('',*,*,#7334,.T.);
#9611=ORIENTED_EDGE('',*,*,#7309,.F.);
#9612=ORIENTED_EDGE('',*,*,#7338,.F.);
#9613=ORIENTED_EDGE('',*,*,#7335,.F.);
#9614=ORIENTED_EDGE('',*,*,#7337,.F.);
#9615=ORIENTED_EDGE('',*,*,#7301,.T.);
#9616=ORIENTED_EDGE('',*,*,#7332,.T.);
#9617=ORIENTED_EDGE('',*,*,#7331,.T.);
#9618=ORIENTED_EDGE('',*,*,#7336,.T.);
#9619=ORIENTED_EDGE('',*,*,#7338,.T.);
#9620=ORIENTED_EDGE('',*,*,#7308,.T.);
#9621=ORIENTED_EDGE('',*,*,#7339,.F.);
#9622=ORIENTED_EDGE('',*,*,#7340,.T.);
#9623=ORIENTED_EDGE('',*,*,#7341,.F.);
#9624=ORIENTED_EDGE('',*,*,#7342,.T.);
#9625=ORIENTED_EDGE('',*,*,#7339,.T.);
#9626=ORIENTED_EDGE('',*,*,#7342,.F.);
#9627=ORIENTED_EDGE('',*,*,#7341,.T.);
#9628=ORIENTED_EDGE('',*,*,#7343,.F.);
#9629=ORIENTED_EDGE('',*,*,#7343,.T.);
#9630=ORIENTED_EDGE('',*,*,#7344,.T.);
#9631=ORIENTED_EDGE('',*,*,#7340,.F.);
#9632=ORIENTED_EDGE('',*,*,#7344,.F.);
#9633=ORIENTED_EDGE('',*,*,#7345,.F.);
#9634=ORIENTED_EDGE('',*,*,#7346,.T.);
#9635=ORIENTED_EDGE('',*,*,#7347,.F.);
#9636=ORIENTED_EDGE('',*,*,#7348,.T.);
#9637=ORIENTED_EDGE('',*,*,#7345,.T.);
#9638=ORIENTED_EDGE('',*,*,#7348,.F.);
#9639=ORIENTED_EDGE('',*,*,#7347,.T.);
#9640=ORIENTED_EDGE('',*,*,#7349,.F.);
#9641=ORIENTED_EDGE('',*,*,#7349,.T.);
#9642=ORIENTED_EDGE('',*,*,#7350,.T.);
#9643=ORIENTED_EDGE('',*,*,#7346,.F.);
#9644=ORIENTED_EDGE('',*,*,#7350,.F.);
#9645=ORIENTED_EDGE('',*,*,#7351,.T.);
#9646=ORIENTED_EDGE('',*,*,#7352,.T.);
#9647=ORIENTED_EDGE('',*,*,#7353,.T.);
#9648=ORIENTED_EDGE('',*,*,#7354,.F.);
#9649=ORIENTED_EDGE('',*,*,#7355,.T.);
#9650=ORIENTED_EDGE('',*,*,#7356,.T.);
#9651=ORIENTED_EDGE('',*,*,#7357,.T.);
#9652=ORIENTED_EDGE('',*,*,#7352,.F.);
#9653=ORIENTED_EDGE('',*,*,#7358,.T.);
#9654=ORIENTED_EDGE('',*,*,#7359,.T.);
#9655=ORIENTED_EDGE('',*,*,#7360,.T.);
#9656=ORIENTED_EDGE('',*,*,#7356,.F.);
#9657=ORIENTED_EDGE('',*,*,#7361,.T.);
#9658=ORIENTED_EDGE('',*,*,#7362,.T.);
#9659=ORIENTED_EDGE('',*,*,#7363,.T.);
#9660=ORIENTED_EDGE('',*,*,#7359,.F.);
#9661=ORIENTED_EDGE('',*,*,#7364,.T.);
#9662=ORIENTED_EDGE('',*,*,#7365,.T.);
#9663=ORIENTED_EDGE('',*,*,#7366,.T.);
#9664=ORIENTED_EDGE('',*,*,#7362,.F.);
#9665=ORIENTED_EDGE('',*,*,#7367,.T.);
#9666=ORIENTED_EDGE('',*,*,#7354,.T.);
#9667=ORIENTED_EDGE('',*,*,#7368,.T.);
#9668=ORIENTED_EDGE('',*,*,#7365,.F.);
#9669=ORIENTED_EDGE('',*,*,#7367,.F.);
#9670=ORIENTED_EDGE('',*,*,#7364,.F.);
#9671=ORIENTED_EDGE('',*,*,#7361,.F.);
#9672=ORIENTED_EDGE('',*,*,#7358,.F.);
#9673=ORIENTED_EDGE('',*,*,#7355,.F.);
#9674=ORIENTED_EDGE('',*,*,#7351,.F.);
#9675=ORIENTED_EDGE('',*,*,#7368,.F.);
#9676=ORIENTED_EDGE('',*,*,#7353,.F.);
#9677=ORIENTED_EDGE('',*,*,#7357,.F.);
#9678=ORIENTED_EDGE('',*,*,#7360,.F.);
#9679=ORIENTED_EDGE('',*,*,#7363,.F.);
#9680=ORIENTED_EDGE('',*,*,#7366,.F.);
#9681=ORIENTED_EDGE('',*,*,#7369,.F.);
#9682=ORIENTED_EDGE('',*,*,#7370,.F.);
#9683=ORIENTED_EDGE('',*,*,#7371,.F.);
#9684=ORIENTED_EDGE('',*,*,#7372,.T.);
#9685=ORIENTED_EDGE('',*,*,#7370,.T.);
#9686=ORIENTED_EDGE('',*,*,#7372,.F.);
#9687=ORIENTED_EDGE('',*,*,#7373,.F.);
#9688=ORIENTED_EDGE('',*,*,#7374,.T.);
#9689=ORIENTED_EDGE('',*,*,#7371,.T.);
#9690=ORIENTED_EDGE('',*,*,#7374,.F.);
#9691=ORIENTED_EDGE('',*,*,#7375,.F.);
#9692=ORIENTED_EDGE('',*,*,#7376,.T.);
#9693=ORIENTED_EDGE('',*,*,#7373,.T.);
#9694=ORIENTED_EDGE('',*,*,#7376,.F.);
#9695=ORIENTED_EDGE('',*,*,#7375,.T.);
#9696=ORIENTED_EDGE('',*,*,#7377,.F.);
#9697=ORIENTED_EDGE('',*,*,#7378,.F.);
#9698=ORIENTED_EDGE('',*,*,#7379,.T.);
#9699=ORIENTED_EDGE('',*,*,#7377,.T.);
#9700=ORIENTED_EDGE('',*,*,#7379,.F.);
#9701=ORIENTED_EDGE('',*,*,#7369,.T.);
#9702=ORIENTED_EDGE('',*,*,#7380,.T.);
#9703=ORIENTED_EDGE('',*,*,#7378,.T.);
#9704=ORIENTED_EDGE('',*,*,#7380,.F.);
#9705=ORIENTED_EDGE('',*,*,#7381,.F.);
#9706=ORIENTED_EDGE('',*,*,#7382,.T.);
#9707=ORIENTED_EDGE('',*,*,#7383,.T.);
#9708=ORIENTED_EDGE('',*,*,#7382,.F.);
#9709=ORIENTED_EDGE('',*,*,#7383,.F.);
#9710=ORIENTED_EDGE('',*,*,#7384,.F.);
#9711=ORIENTED_EDGE('',*,*,#7385,.F.);
#9712=ORIENTED_EDGE('',*,*,#7386,.F.);
#9713=ORIENTED_EDGE('',*,*,#7387,.T.);
#9714=ORIENTED_EDGE('',*,*,#7388,.F.);
#9715=ORIENTED_EDGE('',*,*,#7389,.T.);
#9716=ORIENTED_EDGE('',*,*,#7390,.F.);
#9717=ORIENTED_EDGE('',*,*,#7391,.F.);
#9718=ORIENTED_EDGE('',*,*,#7392,.F.);
#9719=ORIENTED_EDGE('',*,*,#7387,.F.);
#9720=ORIENTED_EDGE('',*,*,#7393,.F.);
#9721=ORIENTED_EDGE('',*,*,#7394,.T.);
#9722=ORIENTED_EDGE('',*,*,#7395,.F.);
#9723=ORIENTED_EDGE('',*,*,#7389,.F.);
#9724=ORIENTED_EDGE('',*,*,#7396,.F.);
#9725=ORIENTED_EDGE('',*,*,#7397,.F.);
#9726=ORIENTED_EDGE('',*,*,#7391,.T.);
#9727=ORIENTED_EDGE('',*,*,#7398,.F.);
#9728=ORIENTED_EDGE('',*,*,#7399,.F.);
#9729=ORIENTED_EDGE('',*,*,#7400,.F.);
#9730=ORIENTED_EDGE('',*,*,#7385,.T.);
#9731=ORIENTED_EDGE('',*,*,#7401,.F.);
#9732=ORIENTED_EDGE('',*,*,#7402,.F.);
#9733=ORIENTED_EDGE('',*,*,#7399,.T.);
#9734=ORIENTED_EDGE('',*,*,#7403,.F.);
#9735=ORIENTED_EDGE('',*,*,#7404,.F.);
#9736=ORIENTED_EDGE('',*,*,#7405,.F.);
#9737=ORIENTED_EDGE('',*,*,#7404,.T.);
#9738=ORIENTED_EDGE('',*,*,#7406,.F.);
#9739=ORIENTED_EDGE('',*,*,#7407,.F.);
#9740=ORIENTED_EDGE('',*,*,#7408,.F.);
#9741=ORIENTED_EDGE('',*,*,#7407,.T.);
#9742=ORIENTED_EDGE('',*,*,#7409,.F.);
#9743=ORIENTED_EDGE('',*,*,#7410,.F.);
#9744=ORIENTED_EDGE('',*,*,#7411,.F.);
#9745=ORIENTED_EDGE('',*,*,#7410,.T.);
#9746=ORIENTED_EDGE('',*,*,#7412,.F.);
#9747=ORIENTED_EDGE('',*,*,#7413,.F.);
#9748=ORIENTED_EDGE('',*,*,#7414,.F.);
#9749=ORIENTED_EDGE('',*,*,#7413,.T.);
#9750=ORIENTED_EDGE('',*,*,#7415,.F.);
#9751=ORIENTED_EDGE('',*,*,#7416,.F.);
#9752=ORIENTED_EDGE('',*,*,#7417,.F.);
#9753=ORIENTED_EDGE('',*,*,#7416,.T.);
#9754=ORIENTED_EDGE('',*,*,#7418,.F.);
#9755=ORIENTED_EDGE('',*,*,#7419,.F.);
#9756=ORIENTED_EDGE('',*,*,#7420,.F.);
#9757=ORIENTED_EDGE('',*,*,#7419,.T.);
#9758=ORIENTED_EDGE('',*,*,#7421,.F.);
#9759=ORIENTED_EDGE('',*,*,#7422,.F.);
#9760=ORIENTED_EDGE('',*,*,#7423,.F.);
#9761=ORIENTED_EDGE('',*,*,#7422,.T.);
#9762=ORIENTED_EDGE('',*,*,#7424,.F.);
#9763=ORIENTED_EDGE('',*,*,#7425,.F.);
#9764=ORIENTED_EDGE('',*,*,#7426,.F.);
#9765=ORIENTED_EDGE('',*,*,#7425,.T.);
#9766=ORIENTED_EDGE('',*,*,#7427,.F.);
#9767=ORIENTED_EDGE('',*,*,#7428,.F.);
#9768=ORIENTED_EDGE('',*,*,#7429,.F.);
#9769=ORIENTED_EDGE('',*,*,#7428,.T.);
#9770=ORIENTED_EDGE('',*,*,#7430,.F.);
#9771=ORIENTED_EDGE('',*,*,#7431,.F.);
#9772=ORIENTED_EDGE('',*,*,#7432,.F.);
#9773=ORIENTED_EDGE('',*,*,#7431,.T.);
#9774=ORIENTED_EDGE('',*,*,#7433,.F.);
#9775=ORIENTED_EDGE('',*,*,#7434,.F.);
#9776=ORIENTED_EDGE('',*,*,#7435,.F.);
#9777=ORIENTED_EDGE('',*,*,#7434,.T.);
#9778=ORIENTED_EDGE('',*,*,#7436,.F.);
#9779=ORIENTED_EDGE('',*,*,#7437,.F.);
#9780=ORIENTED_EDGE('',*,*,#7438,.F.);
#9781=ORIENTED_EDGE('',*,*,#7437,.T.);
#9782=ORIENTED_EDGE('',*,*,#7439,.F.);
#9783=ORIENTED_EDGE('',*,*,#7440,.F.);
#9784=ORIENTED_EDGE('',*,*,#7441,.F.);
#9785=ORIENTED_EDGE('',*,*,#7440,.T.);
#9786=ORIENTED_EDGE('',*,*,#7442,.F.);
#9787=ORIENTED_EDGE('',*,*,#7443,.F.);
#9788=ORIENTED_EDGE('',*,*,#7444,.F.);
#9789=ORIENTED_EDGE('',*,*,#7443,.T.);
#9790=ORIENTED_EDGE('',*,*,#7445,.F.);
#9791=ORIENTED_EDGE('',*,*,#7446,.F.);
#9792=ORIENTED_EDGE('',*,*,#7447,.F.);
#9793=ORIENTED_EDGE('',*,*,#7446,.T.);
#9794=ORIENTED_EDGE('',*,*,#7448,.F.);
#9795=ORIENTED_EDGE('',*,*,#7449,.F.);
#9796=ORIENTED_EDGE('',*,*,#7450,.F.);
#9797=ORIENTED_EDGE('',*,*,#7449,.T.);
#9798=ORIENTED_EDGE('',*,*,#7451,.F.);
#9799=ORIENTED_EDGE('',*,*,#7452,.F.);
#9800=ORIENTED_EDGE('',*,*,#7453,.F.);
#9801=ORIENTED_EDGE('',*,*,#7452,.T.);
#9802=ORIENTED_EDGE('',*,*,#7454,.F.);
#9803=ORIENTED_EDGE('',*,*,#7455,.F.);
#9804=ORIENTED_EDGE('',*,*,#7456,.F.);
#9805=ORIENTED_EDGE('',*,*,#7455,.T.);
#9806=ORIENTED_EDGE('',*,*,#7457,.F.);
#9807=ORIENTED_EDGE('',*,*,#7458,.F.);
#9808=ORIENTED_EDGE('',*,*,#7459,.F.);
#9809=ORIENTED_EDGE('',*,*,#7458,.T.);
#9810=ORIENTED_EDGE('',*,*,#7460,.F.);
#9811=ORIENTED_EDGE('',*,*,#7461,.F.);
#9812=ORIENTED_EDGE('',*,*,#7462,.F.);
#9813=ORIENTED_EDGE('',*,*,#7461,.T.);
#9814=ORIENTED_EDGE('',*,*,#7463,.F.);
#9815=ORIENTED_EDGE('',*,*,#7464,.F.);
#9816=ORIENTED_EDGE('',*,*,#7465,.F.);
#9817=ORIENTED_EDGE('',*,*,#7464,.T.);
#9818=ORIENTED_EDGE('',*,*,#7466,.F.);
#9819=ORIENTED_EDGE('',*,*,#7467,.F.);
#9820=ORIENTED_EDGE('',*,*,#7468,.F.);
#9821=ORIENTED_EDGE('',*,*,#7467,.T.);
#9822=ORIENTED_EDGE('',*,*,#7469,.F.);
#9823=ORIENTED_EDGE('',*,*,#7470,.F.);
#9824=ORIENTED_EDGE('',*,*,#7471,.F.);
#9825=ORIENTED_EDGE('',*,*,#7470,.T.);
#9826=ORIENTED_EDGE('',*,*,#7472,.F.);
#9827=ORIENTED_EDGE('',*,*,#7473,.F.);
#9828=ORIENTED_EDGE('',*,*,#7474,.F.);
#9829=ORIENTED_EDGE('',*,*,#7473,.T.);
#9830=ORIENTED_EDGE('',*,*,#7475,.F.);
#9831=ORIENTED_EDGE('',*,*,#7476,.F.);
#9832=ORIENTED_EDGE('',*,*,#7477,.F.);
#9833=ORIENTED_EDGE('',*,*,#7476,.T.);
#9834=ORIENTED_EDGE('',*,*,#7478,.F.);
#9835=ORIENTED_EDGE('',*,*,#7479,.F.);
#9836=ORIENTED_EDGE('',*,*,#7480,.F.);
#9837=ORIENTED_EDGE('',*,*,#7479,.T.);
#9838=ORIENTED_EDGE('',*,*,#7481,.F.);
#9839=ORIENTED_EDGE('',*,*,#7482,.F.);
#9840=ORIENTED_EDGE('',*,*,#7483,.F.);
#9841=ORIENTED_EDGE('',*,*,#7482,.T.);
#9842=ORIENTED_EDGE('',*,*,#7484,.F.);
#9843=ORIENTED_EDGE('',*,*,#7485,.F.);
#9844=ORIENTED_EDGE('',*,*,#7486,.F.);
#9845=ORIENTED_EDGE('',*,*,#7485,.T.);
#9846=ORIENTED_EDGE('',*,*,#7487,.F.);
#9847=ORIENTED_EDGE('',*,*,#7488,.F.);
#9848=ORIENTED_EDGE('',*,*,#7489,.F.);
#9849=ORIENTED_EDGE('',*,*,#7488,.T.);
#9850=ORIENTED_EDGE('',*,*,#7490,.F.);
#9851=ORIENTED_EDGE('',*,*,#7491,.F.);
#9852=ORIENTED_EDGE('',*,*,#7492,.F.);
#9853=ORIENTED_EDGE('',*,*,#7491,.T.);
#9854=ORIENTED_EDGE('',*,*,#7493,.F.);
#9855=ORIENTED_EDGE('',*,*,#7494,.F.);
#9856=ORIENTED_EDGE('',*,*,#7495,.F.);
#9857=ORIENTED_EDGE('',*,*,#7494,.T.);
#9858=ORIENTED_EDGE('',*,*,#7496,.F.);
#9859=ORIENTED_EDGE('',*,*,#7497,.F.);
#9860=ORIENTED_EDGE('',*,*,#7498,.F.);
#9861=ORIENTED_EDGE('',*,*,#7497,.T.);
#9862=ORIENTED_EDGE('',*,*,#7499,.F.);
#9863=ORIENTED_EDGE('',*,*,#7500,.F.);
#9864=ORIENTED_EDGE('',*,*,#7501,.F.);
#9865=ORIENTED_EDGE('',*,*,#7500,.T.);
#9866=ORIENTED_EDGE('',*,*,#7502,.F.);
#9867=ORIENTED_EDGE('',*,*,#7503,.F.);
#9868=ORIENTED_EDGE('',*,*,#7504,.F.);
#9869=ORIENTED_EDGE('',*,*,#7503,.T.);
#9870=ORIENTED_EDGE('',*,*,#7505,.F.);
#9871=ORIENTED_EDGE('',*,*,#7506,.F.);
#9872=ORIENTED_EDGE('',*,*,#7507,.F.);
#9873=ORIENTED_EDGE('',*,*,#7506,.T.);
#9874=ORIENTED_EDGE('',*,*,#7508,.F.);
#9875=ORIENTED_EDGE('',*,*,#7509,.F.);
#9876=ORIENTED_EDGE('',*,*,#7510,.F.);
#9877=ORIENTED_EDGE('',*,*,#7509,.T.);
#9878=ORIENTED_EDGE('',*,*,#7511,.F.);
#9879=ORIENTED_EDGE('',*,*,#7512,.F.);
#9880=ORIENTED_EDGE('',*,*,#7513,.F.);
#9881=ORIENTED_EDGE('',*,*,#7512,.T.);
#9882=ORIENTED_EDGE('',*,*,#7514,.F.);
#9883=ORIENTED_EDGE('',*,*,#7515,.F.);
#9884=ORIENTED_EDGE('',*,*,#7516,.F.);
#9885=ORIENTED_EDGE('',*,*,#7515,.T.);
#9886=ORIENTED_EDGE('',*,*,#7517,.F.);
#9887=ORIENTED_EDGE('',*,*,#7518,.F.);
#9888=ORIENTED_EDGE('',*,*,#7519,.F.);
#9889=ORIENTED_EDGE('',*,*,#7518,.T.);
#9890=ORIENTED_EDGE('',*,*,#7520,.F.);
#9891=ORIENTED_EDGE('',*,*,#7521,.F.);
#9892=ORIENTED_EDGE('',*,*,#7522,.F.);
#9893=ORIENTED_EDGE('',*,*,#7521,.T.);
#9894=ORIENTED_EDGE('',*,*,#7523,.F.);
#9895=ORIENTED_EDGE('',*,*,#7524,.F.);
#9896=ORIENTED_EDGE('',*,*,#7525,.F.);
#9897=ORIENTED_EDGE('',*,*,#7524,.T.);
#9898=ORIENTED_EDGE('',*,*,#7526,.F.);
#9899=ORIENTED_EDGE('',*,*,#7527,.F.);
#9900=ORIENTED_EDGE('',*,*,#7528,.F.);
#9901=ORIENTED_EDGE('',*,*,#7527,.T.);
#9902=ORIENTED_EDGE('',*,*,#7529,.F.);
#9903=ORIENTED_EDGE('',*,*,#7530,.F.);
#9904=ORIENTED_EDGE('',*,*,#7531,.F.);
#9905=ORIENTED_EDGE('',*,*,#7530,.T.);
#9906=ORIENTED_EDGE('',*,*,#7532,.F.);
#9907=ORIENTED_EDGE('',*,*,#7533,.F.);
#9908=ORIENTED_EDGE('',*,*,#7534,.F.);
#9909=ORIENTED_EDGE('',*,*,#7533,.T.);
#9910=ORIENTED_EDGE('',*,*,#7535,.F.);
#9911=ORIENTED_EDGE('',*,*,#7536,.F.);
#9912=ORIENTED_EDGE('',*,*,#7537,.F.);
#9913=ORIENTED_EDGE('',*,*,#7536,.T.);
#9914=ORIENTED_EDGE('',*,*,#7538,.F.);
#9915=ORIENTED_EDGE('',*,*,#7539,.F.);
#9916=ORIENTED_EDGE('',*,*,#7540,.F.);
#9917=ORIENTED_EDGE('',*,*,#7539,.T.);
#9918=ORIENTED_EDGE('',*,*,#7541,.F.);
#9919=ORIENTED_EDGE('',*,*,#7542,.F.);
#9920=ORIENTED_EDGE('',*,*,#7543,.F.);
#9921=ORIENTED_EDGE('',*,*,#7542,.T.);
#9922=ORIENTED_EDGE('',*,*,#7544,.F.);
#9923=ORIENTED_EDGE('',*,*,#7545,.F.);
#9924=ORIENTED_EDGE('',*,*,#7546,.F.);
#9925=ORIENTED_EDGE('',*,*,#7545,.T.);
#9926=ORIENTED_EDGE('',*,*,#7547,.F.);
#9927=ORIENTED_EDGE('',*,*,#7548,.F.);
#9928=ORIENTED_EDGE('',*,*,#7549,.F.);
#9929=ORIENTED_EDGE('',*,*,#7548,.T.);
#9930=ORIENTED_EDGE('',*,*,#7550,.F.);
#9931=ORIENTED_EDGE('',*,*,#7551,.F.);
#9932=ORIENTED_EDGE('',*,*,#7552,.F.);
#9933=ORIENTED_EDGE('',*,*,#7551,.T.);
#9934=ORIENTED_EDGE('',*,*,#7553,.F.);
#9935=ORIENTED_EDGE('',*,*,#7554,.F.);
#9936=ORIENTED_EDGE('',*,*,#7555,.F.);
#9937=ORIENTED_EDGE('',*,*,#7554,.T.);
#9938=ORIENTED_EDGE('',*,*,#7556,.F.);
#9939=ORIENTED_EDGE('',*,*,#7557,.F.);
#9940=ORIENTED_EDGE('',*,*,#7558,.F.);
#9941=ORIENTED_EDGE('',*,*,#7557,.T.);
#9942=ORIENTED_EDGE('',*,*,#7559,.F.);
#9943=ORIENTED_EDGE('',*,*,#7560,.F.);
#9944=ORIENTED_EDGE('',*,*,#7561,.F.);
#9945=ORIENTED_EDGE('',*,*,#7560,.T.);
#9946=ORIENTED_EDGE('',*,*,#7562,.F.);
#9947=ORIENTED_EDGE('',*,*,#7563,.F.);
#9948=ORIENTED_EDGE('',*,*,#7564,.F.);
#9949=ORIENTED_EDGE('',*,*,#7563,.T.);
#9950=ORIENTED_EDGE('',*,*,#7565,.F.);
#9951=ORIENTED_EDGE('',*,*,#7566,.F.);
#9952=ORIENTED_EDGE('',*,*,#7567,.F.);
#9953=ORIENTED_EDGE('',*,*,#7566,.T.);
#9954=ORIENTED_EDGE('',*,*,#7568,.F.);
#9955=ORIENTED_EDGE('',*,*,#7569,.F.);
#9956=ORIENTED_EDGE('',*,*,#7570,.F.);
#9957=ORIENTED_EDGE('',*,*,#7569,.T.);
#9958=ORIENTED_EDGE('',*,*,#7571,.F.);
#9959=ORIENTED_EDGE('',*,*,#7572,.F.);
#9960=ORIENTED_EDGE('',*,*,#7573,.F.);
#9961=ORIENTED_EDGE('',*,*,#7572,.T.);
#9962=ORIENTED_EDGE('',*,*,#7574,.F.);
#9963=ORIENTED_EDGE('',*,*,#7575,.F.);
#9964=ORIENTED_EDGE('',*,*,#7576,.F.);
#9965=ORIENTED_EDGE('',*,*,#7575,.T.);
#9966=ORIENTED_EDGE('',*,*,#7577,.F.);
#9967=ORIENTED_EDGE('',*,*,#7578,.F.);
#9968=ORIENTED_EDGE('',*,*,#7579,.F.);
#9969=ORIENTED_EDGE('',*,*,#7578,.T.);
#9970=ORIENTED_EDGE('',*,*,#7580,.F.);
#9971=ORIENTED_EDGE('',*,*,#7581,.F.);
#9972=ORIENTED_EDGE('',*,*,#7582,.F.);
#9973=ORIENTED_EDGE('',*,*,#7581,.T.);
#9974=ORIENTED_EDGE('',*,*,#7583,.F.);
#9975=ORIENTED_EDGE('',*,*,#7584,.F.);
#9976=ORIENTED_EDGE('',*,*,#7585,.F.);
#9977=ORIENTED_EDGE('',*,*,#7584,.T.);
#9978=ORIENTED_EDGE('',*,*,#7586,.F.);
#9979=ORIENTED_EDGE('',*,*,#7587,.F.);
#9980=ORIENTED_EDGE('',*,*,#7588,.F.);
#9981=ORIENTED_EDGE('',*,*,#7587,.T.);
#9982=ORIENTED_EDGE('',*,*,#7589,.F.);
#9983=ORIENTED_EDGE('',*,*,#7590,.F.);
#9984=ORIENTED_EDGE('',*,*,#7591,.F.);
#9985=ORIENTED_EDGE('',*,*,#7590,.T.);
#9986=ORIENTED_EDGE('',*,*,#7592,.F.);
#9987=ORIENTED_EDGE('',*,*,#7593,.F.);
#9988=ORIENTED_EDGE('',*,*,#7594,.F.);
#9989=ORIENTED_EDGE('',*,*,#7593,.T.);
#9990=ORIENTED_EDGE('',*,*,#7595,.F.);
#9991=ORIENTED_EDGE('',*,*,#7596,.F.);
#9992=ORIENTED_EDGE('',*,*,#7597,.F.);
#9993=ORIENTED_EDGE('',*,*,#7596,.T.);
#9994=ORIENTED_EDGE('',*,*,#7598,.F.);
#9995=ORIENTED_EDGE('',*,*,#7599,.F.);
#9996=ORIENTED_EDGE('',*,*,#7600,.F.);
#9997=ORIENTED_EDGE('',*,*,#7599,.T.);
#9998=ORIENTED_EDGE('',*,*,#7601,.F.);
#9999=ORIENTED_EDGE('',*,*,#7602,.F.);
#10000=ORIENTED_EDGE('',*,*,#7603,.F.);
#10001=ORIENTED_EDGE('',*,*,#7602,.T.);
#10002=ORIENTED_EDGE('',*,*,#7604,.F.);
#10003=ORIENTED_EDGE('',*,*,#7605,.F.);
#10004=ORIENTED_EDGE('',*,*,#7606,.F.);
#10005=ORIENTED_EDGE('',*,*,#7605,.T.);
#10006=ORIENTED_EDGE('',*,*,#7607,.F.);
#10007=ORIENTED_EDGE('',*,*,#7608,.F.);
#10008=ORIENTED_EDGE('',*,*,#7609,.F.);
#10009=ORIENTED_EDGE('',*,*,#7608,.T.);
#10010=ORIENTED_EDGE('',*,*,#7610,.F.);
#10011=ORIENTED_EDGE('',*,*,#7611,.F.);
#10012=ORIENTED_EDGE('',*,*,#7612,.F.);
#10013=ORIENTED_EDGE('',*,*,#7611,.T.);
#10014=ORIENTED_EDGE('',*,*,#7613,.F.);
#10015=ORIENTED_EDGE('',*,*,#7614,.F.);
#10016=ORIENTED_EDGE('',*,*,#7615,.F.);
#10017=ORIENTED_EDGE('',*,*,#7614,.T.);
#10018=ORIENTED_EDGE('',*,*,#7616,.F.);
#10019=ORIENTED_EDGE('',*,*,#7617,.F.);
#10020=ORIENTED_EDGE('',*,*,#7618,.F.);
#10021=ORIENTED_EDGE('',*,*,#7617,.T.);
#10022=ORIENTED_EDGE('',*,*,#7619,.F.);
#10023=ORIENTED_EDGE('',*,*,#7620,.F.);
#10024=ORIENTED_EDGE('',*,*,#7621,.F.);
#10025=ORIENTED_EDGE('',*,*,#7620,.T.);
#10026=ORIENTED_EDGE('',*,*,#7622,.F.);
#10027=ORIENTED_EDGE('',*,*,#7623,.F.);
#10028=ORIENTED_EDGE('',*,*,#7624,.F.);
#10029=ORIENTED_EDGE('',*,*,#7623,.T.);
#10030=ORIENTED_EDGE('',*,*,#7625,.F.);
#10031=ORIENTED_EDGE('',*,*,#7626,.F.);
#10032=ORIENTED_EDGE('',*,*,#7627,.F.);
#10033=ORIENTED_EDGE('',*,*,#7626,.T.);
#10034=ORIENTED_EDGE('',*,*,#7628,.F.);
#10035=ORIENTED_EDGE('',*,*,#7629,.F.);
#10036=ORIENTED_EDGE('',*,*,#7630,.F.);
#10037=ORIENTED_EDGE('',*,*,#7629,.T.);
#10038=ORIENTED_EDGE('',*,*,#7631,.F.);
#10039=ORIENTED_EDGE('',*,*,#7632,.F.);
#10040=ORIENTED_EDGE('',*,*,#7633,.F.);
#10041=ORIENTED_EDGE('',*,*,#7632,.T.);
#10042=ORIENTED_EDGE('',*,*,#7634,.F.);
#10043=ORIENTED_EDGE('',*,*,#7635,.F.);
#10044=ORIENTED_EDGE('',*,*,#7636,.F.);
#10045=ORIENTED_EDGE('',*,*,#7635,.T.);
#10046=ORIENTED_EDGE('',*,*,#7637,.F.);
#10047=ORIENTED_EDGE('',*,*,#7638,.F.);
#10048=ORIENTED_EDGE('',*,*,#7639,.F.);
#10049=ORIENTED_EDGE('',*,*,#7638,.T.);
#10050=ORIENTED_EDGE('',*,*,#7640,.F.);
#10051=ORIENTED_EDGE('',*,*,#7641,.F.);
#10052=ORIENTED_EDGE('',*,*,#7642,.F.);
#10053=ORIENTED_EDGE('',*,*,#7641,.T.);
#10054=ORIENTED_EDGE('',*,*,#7643,.F.);
#10055=ORIENTED_EDGE('',*,*,#7644,.F.);
#10056=ORIENTED_EDGE('',*,*,#7645,.F.);
#10057=ORIENTED_EDGE('',*,*,#7644,.T.);
#10058=ORIENTED_EDGE('',*,*,#7646,.F.);
#10059=ORIENTED_EDGE('',*,*,#7647,.F.);
#10060=ORIENTED_EDGE('',*,*,#7648,.F.);
#10061=ORIENTED_EDGE('',*,*,#7647,.T.);
#10062=ORIENTED_EDGE('',*,*,#7649,.F.);
#10063=ORIENTED_EDGE('',*,*,#7650,.F.);
#10064=ORIENTED_EDGE('',*,*,#7651,.F.);
#10065=ORIENTED_EDGE('',*,*,#7650,.T.);
#10066=ORIENTED_EDGE('',*,*,#7652,.F.);
#10067=ORIENTED_EDGE('',*,*,#7653,.F.);
#10068=ORIENTED_EDGE('',*,*,#7654,.F.);
#10069=ORIENTED_EDGE('',*,*,#7653,.T.);
#10070=ORIENTED_EDGE('',*,*,#7655,.F.);
#10071=ORIENTED_EDGE('',*,*,#7656,.F.);
#10072=ORIENTED_EDGE('',*,*,#7657,.F.);
#10073=ORIENTED_EDGE('',*,*,#7656,.T.);
#10074=ORIENTED_EDGE('',*,*,#7658,.F.);
#10075=ORIENTED_EDGE('',*,*,#7659,.F.);
#10076=ORIENTED_EDGE('',*,*,#7660,.F.);
#10077=ORIENTED_EDGE('',*,*,#7659,.T.);
#10078=ORIENTED_EDGE('',*,*,#7661,.F.);
#10079=ORIENTED_EDGE('',*,*,#7662,.F.);
#10080=ORIENTED_EDGE('',*,*,#7663,.F.);
#10081=ORIENTED_EDGE('',*,*,#7662,.T.);
#10082=ORIENTED_EDGE('',*,*,#7664,.F.);
#10083=ORIENTED_EDGE('',*,*,#7665,.F.);
#10084=ORIENTED_EDGE('',*,*,#7666,.F.);
#10085=ORIENTED_EDGE('',*,*,#7665,.T.);
#10086=ORIENTED_EDGE('',*,*,#7667,.F.);
#10087=ORIENTED_EDGE('',*,*,#7668,.F.);
#10088=ORIENTED_EDGE('',*,*,#7669,.F.);
#10089=ORIENTED_EDGE('',*,*,#7668,.T.);
#10090=ORIENTED_EDGE('',*,*,#7670,.F.);
#10091=ORIENTED_EDGE('',*,*,#7671,.F.);
#10092=ORIENTED_EDGE('',*,*,#7672,.F.);
#10093=ORIENTED_EDGE('',*,*,#7671,.T.);
#10094=ORIENTED_EDGE('',*,*,#7673,.F.);
#10095=ORIENTED_EDGE('',*,*,#7674,.F.);
#10096=ORIENTED_EDGE('',*,*,#7675,.F.);
#10097=ORIENTED_EDGE('',*,*,#7674,.T.);
#10098=ORIENTED_EDGE('',*,*,#7676,.F.);
#10099=ORIENTED_EDGE('',*,*,#7677,.F.);
#10100=ORIENTED_EDGE('',*,*,#7678,.F.);
#10101=ORIENTED_EDGE('',*,*,#7677,.T.);
#10102=ORIENTED_EDGE('',*,*,#7679,.F.);
#10103=ORIENTED_EDGE('',*,*,#7680,.F.);
#10104=ORIENTED_EDGE('',*,*,#7681,.F.);
#10105=ORIENTED_EDGE('',*,*,#7680,.T.);
#10106=ORIENTED_EDGE('',*,*,#7682,.F.);
#10107=ORIENTED_EDGE('',*,*,#7683,.F.);
#10108=ORIENTED_EDGE('',*,*,#7684,.F.);
#10109=ORIENTED_EDGE('',*,*,#7683,.T.);
#10110=ORIENTED_EDGE('',*,*,#7685,.F.);
#10111=ORIENTED_EDGE('',*,*,#7686,.F.);
#10112=ORIENTED_EDGE('',*,*,#7687,.F.);
#10113=ORIENTED_EDGE('',*,*,#7686,.T.);
#10114=ORIENTED_EDGE('',*,*,#7688,.F.);
#10115=ORIENTED_EDGE('',*,*,#7689,.F.);
#10116=ORIENTED_EDGE('',*,*,#7690,.F.);
#10117=ORIENTED_EDGE('',*,*,#7689,.T.);
#10118=ORIENTED_EDGE('',*,*,#7691,.F.);
#10119=ORIENTED_EDGE('',*,*,#7692,.F.);
#10120=ORIENTED_EDGE('',*,*,#7693,.F.);
#10121=ORIENTED_EDGE('',*,*,#7692,.T.);
#10122=ORIENTED_EDGE('',*,*,#7694,.F.);
#10123=ORIENTED_EDGE('',*,*,#7695,.F.);
#10124=ORIENTED_EDGE('',*,*,#7696,.F.);
#10125=ORIENTED_EDGE('',*,*,#7695,.T.);
#10126=ORIENTED_EDGE('',*,*,#7697,.F.);
#10127=ORIENTED_EDGE('',*,*,#7698,.F.);
#10128=ORIENTED_EDGE('',*,*,#7699,.F.);
#10129=ORIENTED_EDGE('',*,*,#7698,.T.);
#10130=ORIENTED_EDGE('',*,*,#7700,.F.);
#10131=ORIENTED_EDGE('',*,*,#7701,.F.);
#10132=ORIENTED_EDGE('',*,*,#7702,.F.);
#10133=ORIENTED_EDGE('',*,*,#7701,.T.);
#10134=ORIENTED_EDGE('',*,*,#7703,.F.);
#10135=ORIENTED_EDGE('',*,*,#7704,.F.);
#10136=ORIENTED_EDGE('',*,*,#7705,.F.);
#10137=ORIENTED_EDGE('',*,*,#7704,.T.);
#10138=ORIENTED_EDGE('',*,*,#7706,.F.);
#10139=ORIENTED_EDGE('',*,*,#7707,.F.);
#10140=ORIENTED_EDGE('',*,*,#7708,.F.);
#10141=ORIENTED_EDGE('',*,*,#7707,.T.);
#10142=ORIENTED_EDGE('',*,*,#7709,.F.);
#10143=ORIENTED_EDGE('',*,*,#7710,.F.);
#10144=ORIENTED_EDGE('',*,*,#7711,.F.);
#10145=ORIENTED_EDGE('',*,*,#7710,.T.);
#10146=ORIENTED_EDGE('',*,*,#7712,.F.);
#10147=ORIENTED_EDGE('',*,*,#7713,.F.);
#10148=ORIENTED_EDGE('',*,*,#7714,.F.);
#10149=ORIENTED_EDGE('',*,*,#7713,.T.);
#10150=ORIENTED_EDGE('',*,*,#7715,.F.);
#10151=ORIENTED_EDGE('',*,*,#7716,.F.);
#10152=ORIENTED_EDGE('',*,*,#7717,.F.);
#10153=ORIENTED_EDGE('',*,*,#7716,.T.);
#10154=ORIENTED_EDGE('',*,*,#7718,.F.);
#10155=ORIENTED_EDGE('',*,*,#7719,.F.);
#10156=ORIENTED_EDGE('',*,*,#7720,.F.);
#10157=ORIENTED_EDGE('',*,*,#7719,.T.);
#10158=ORIENTED_EDGE('',*,*,#7721,.F.);
#10159=ORIENTED_EDGE('',*,*,#7722,.F.);
#10160=ORIENTED_EDGE('',*,*,#7723,.F.);
#10161=ORIENTED_EDGE('',*,*,#7722,.T.);
#10162=ORIENTED_EDGE('',*,*,#7724,.F.);
#10163=ORIENTED_EDGE('',*,*,#7725,.F.);
#10164=ORIENTED_EDGE('',*,*,#7726,.F.);
#10165=ORIENTED_EDGE('',*,*,#7725,.T.);
#10166=ORIENTED_EDGE('',*,*,#7727,.F.);
#10167=ORIENTED_EDGE('',*,*,#7728,.F.);
#10168=ORIENTED_EDGE('',*,*,#7729,.F.);
#10169=ORIENTED_EDGE('',*,*,#7728,.T.);
#10170=ORIENTED_EDGE('',*,*,#7730,.F.);
#10171=ORIENTED_EDGE('',*,*,#7731,.F.);
#10172=ORIENTED_EDGE('',*,*,#7732,.F.);
#10173=ORIENTED_EDGE('',*,*,#7731,.T.);
#10174=ORIENTED_EDGE('',*,*,#7733,.F.);
#10175=ORIENTED_EDGE('',*,*,#7734,.F.);
#10176=ORIENTED_EDGE('',*,*,#7735,.F.);
#10177=ORIENTED_EDGE('',*,*,#7734,.T.);
#10178=ORIENTED_EDGE('',*,*,#7736,.F.);
#10179=ORIENTED_EDGE('',*,*,#7737,.F.);
#10180=ORIENTED_EDGE('',*,*,#7738,.F.);
#10181=ORIENTED_EDGE('',*,*,#7737,.T.);
#10182=ORIENTED_EDGE('',*,*,#7739,.F.);
#10183=ORIENTED_EDGE('',*,*,#7740,.F.);
#10184=ORIENTED_EDGE('',*,*,#7741,.F.);
#10185=ORIENTED_EDGE('',*,*,#7740,.T.);
#10186=ORIENTED_EDGE('',*,*,#7742,.F.);
#10187=ORIENTED_EDGE('',*,*,#7743,.F.);
#10188=ORIENTED_EDGE('',*,*,#7744,.F.);
#10189=ORIENTED_EDGE('',*,*,#7743,.T.);
#10190=ORIENTED_EDGE('',*,*,#7745,.F.);
#10191=ORIENTED_EDGE('',*,*,#7746,.F.);
#10192=ORIENTED_EDGE('',*,*,#7747,.F.);
#10193=ORIENTED_EDGE('',*,*,#7746,.T.);
#10194=ORIENTED_EDGE('',*,*,#7748,.F.);
#10195=ORIENTED_EDGE('',*,*,#7749,.F.);
#10196=ORIENTED_EDGE('',*,*,#7750,.F.);
#10197=ORIENTED_EDGE('',*,*,#7749,.T.);
#10198=ORIENTED_EDGE('',*,*,#7751,.F.);
#10199=ORIENTED_EDGE('',*,*,#7752,.F.);
#10200=ORIENTED_EDGE('',*,*,#7753,.F.);
#10201=ORIENTED_EDGE('',*,*,#7752,.T.);
#10202=ORIENTED_EDGE('',*,*,#7754,.F.);
#10203=ORIENTED_EDGE('',*,*,#7755,.F.);
#10204=ORIENTED_EDGE('',*,*,#7756,.F.);
#10205=ORIENTED_EDGE('',*,*,#7755,.T.);
#10206=ORIENTED_EDGE('',*,*,#7757,.F.);
#10207=ORIENTED_EDGE('',*,*,#7758,.F.);
#10208=ORIENTED_EDGE('',*,*,#7759,.F.);
#10209=ORIENTED_EDGE('',*,*,#7758,.T.);
#10210=ORIENTED_EDGE('',*,*,#7760,.F.);
#10211=ORIENTED_EDGE('',*,*,#7761,.F.);
#10212=ORIENTED_EDGE('',*,*,#7762,.F.);
#10213=ORIENTED_EDGE('',*,*,#7761,.T.);
#10214=ORIENTED_EDGE('',*,*,#7763,.F.);
#10215=ORIENTED_EDGE('',*,*,#7764,.F.);
#10216=ORIENTED_EDGE('',*,*,#7765,.F.);
#10217=ORIENTED_EDGE('',*,*,#7764,.T.);
#10218=ORIENTED_EDGE('',*,*,#7766,.F.);
#10219=ORIENTED_EDGE('',*,*,#7767,.F.);
#10220=ORIENTED_EDGE('',*,*,#7768,.F.);
#10221=ORIENTED_EDGE('',*,*,#7767,.T.);
#10222=ORIENTED_EDGE('',*,*,#7769,.F.);
#10223=ORIENTED_EDGE('',*,*,#7770,.F.);
#10224=ORIENTED_EDGE('',*,*,#7771,.F.);
#10225=ORIENTED_EDGE('',*,*,#7770,.T.);
#10226=ORIENTED_EDGE('',*,*,#7772,.F.);
#10227=ORIENTED_EDGE('',*,*,#7773,.F.);
#10228=ORIENTED_EDGE('',*,*,#7774,.F.);
#10229=ORIENTED_EDGE('',*,*,#7773,.T.);
#10230=ORIENTED_EDGE('',*,*,#7775,.F.);
#10231=ORIENTED_EDGE('',*,*,#7776,.F.);
#10232=ORIENTED_EDGE('',*,*,#7777,.F.);
#10233=ORIENTED_EDGE('',*,*,#7776,.T.);
#10234=ORIENTED_EDGE('',*,*,#7778,.F.);
#10235=ORIENTED_EDGE('',*,*,#7779,.F.);
#10236=ORIENTED_EDGE('',*,*,#7780,.F.);
#10237=ORIENTED_EDGE('',*,*,#7779,.T.);
#10238=ORIENTED_EDGE('',*,*,#7781,.F.);
#10239=ORIENTED_EDGE('',*,*,#7782,.F.);
#10240=ORIENTED_EDGE('',*,*,#7783,.F.);
#10241=ORIENTED_EDGE('',*,*,#7782,.T.);
#10242=ORIENTED_EDGE('',*,*,#7784,.F.);
#10243=ORIENTED_EDGE('',*,*,#7785,.F.);
#10244=ORIENTED_EDGE('',*,*,#7786,.F.);
#10245=ORIENTED_EDGE('',*,*,#7785,.T.);
#10246=ORIENTED_EDGE('',*,*,#7787,.F.);
#10247=ORIENTED_EDGE('',*,*,#7788,.F.);
#10248=ORIENTED_EDGE('',*,*,#7789,.F.);
#10249=ORIENTED_EDGE('',*,*,#7788,.T.);
#10250=ORIENTED_EDGE('',*,*,#7790,.F.);
#10251=ORIENTED_EDGE('',*,*,#7791,.F.);
#10252=ORIENTED_EDGE('',*,*,#7792,.F.);
#10253=ORIENTED_EDGE('',*,*,#7791,.T.);
#10254=ORIENTED_EDGE('',*,*,#7793,.F.);
#10255=ORIENTED_EDGE('',*,*,#7794,.F.);
#10256=ORIENTED_EDGE('',*,*,#7795,.F.);
#10257=ORIENTED_EDGE('',*,*,#7794,.T.);
#10258=ORIENTED_EDGE('',*,*,#7796,.F.);
#10259=ORIENTED_EDGE('',*,*,#7797,.F.);
#10260=ORIENTED_EDGE('',*,*,#7798,.F.);
#10261=ORIENTED_EDGE('',*,*,#7797,.T.);
#10262=ORIENTED_EDGE('',*,*,#7799,.F.);
#10263=ORIENTED_EDGE('',*,*,#7800,.F.);
#10264=ORIENTED_EDGE('',*,*,#7801,.F.);
#10265=ORIENTED_EDGE('',*,*,#7800,.T.);
#10266=ORIENTED_EDGE('',*,*,#7802,.F.);
#10267=ORIENTED_EDGE('',*,*,#7803,.F.);
#10268=ORIENTED_EDGE('',*,*,#7804,.F.);
#10269=ORIENTED_EDGE('',*,*,#7803,.T.);
#10270=ORIENTED_EDGE('',*,*,#7805,.F.);
#10271=ORIENTED_EDGE('',*,*,#7806,.F.);
#10272=ORIENTED_EDGE('',*,*,#7807,.F.);
#10273=ORIENTED_EDGE('',*,*,#7806,.T.);
#10274=ORIENTED_EDGE('',*,*,#7808,.F.);
#10275=ORIENTED_EDGE('',*,*,#7809,.F.);
#10276=ORIENTED_EDGE('',*,*,#7810,.F.);
#10277=ORIENTED_EDGE('',*,*,#7809,.T.);
#10278=ORIENTED_EDGE('',*,*,#7811,.F.);
#10279=ORIENTED_EDGE('',*,*,#7812,.F.);
#10280=ORIENTED_EDGE('',*,*,#7813,.F.);
#10281=ORIENTED_EDGE('',*,*,#7812,.T.);
#10282=ORIENTED_EDGE('',*,*,#7814,.F.);
#10283=ORIENTED_EDGE('',*,*,#7815,.F.);
#10284=ORIENTED_EDGE('',*,*,#7816,.F.);
#10285=ORIENTED_EDGE('',*,*,#7815,.T.);
#10286=ORIENTED_EDGE('',*,*,#7817,.F.);
#10287=ORIENTED_EDGE('',*,*,#7818,.F.);
#10288=ORIENTED_EDGE('',*,*,#7819,.F.);
#10289=ORIENTED_EDGE('',*,*,#7818,.T.);
#10290=ORIENTED_EDGE('',*,*,#7820,.F.);
#10291=ORIENTED_EDGE('',*,*,#7821,.F.);
#10292=ORIENTED_EDGE('',*,*,#7822,.F.);
#10293=ORIENTED_EDGE('',*,*,#7821,.T.);
#10294=ORIENTED_EDGE('',*,*,#7823,.F.);
#10295=ORIENTED_EDGE('',*,*,#7824,.F.);
#10296=ORIENTED_EDGE('',*,*,#7825,.F.);
#10297=ORIENTED_EDGE('',*,*,#7824,.T.);
#10298=ORIENTED_EDGE('',*,*,#7826,.F.);
#10299=ORIENTED_EDGE('',*,*,#7827,.F.);
#10300=ORIENTED_EDGE('',*,*,#7828,.F.);
#10301=ORIENTED_EDGE('',*,*,#7827,.T.);
#10302=ORIENTED_EDGE('',*,*,#7829,.F.);
#10303=ORIENTED_EDGE('',*,*,#7830,.F.);
#10304=ORIENTED_EDGE('',*,*,#7831,.F.);
#10305=ORIENTED_EDGE('',*,*,#7830,.T.);
#10306=ORIENTED_EDGE('',*,*,#7832,.F.);
#10307=ORIENTED_EDGE('',*,*,#7833,.F.);
#10308=ORIENTED_EDGE('',*,*,#7834,.F.);
#10309=ORIENTED_EDGE('',*,*,#7833,.T.);
#10310=ORIENTED_EDGE('',*,*,#7835,.F.);
#10311=ORIENTED_EDGE('',*,*,#7836,.F.);
#10312=ORIENTED_EDGE('',*,*,#7837,.F.);
#10313=ORIENTED_EDGE('',*,*,#7836,.T.);
#10314=ORIENTED_EDGE('',*,*,#7838,.F.);
#10315=ORIENTED_EDGE('',*,*,#7839,.F.);
#10316=ORIENTED_EDGE('',*,*,#7840,.F.);
#10317=ORIENTED_EDGE('',*,*,#7839,.T.);
#10318=ORIENTED_EDGE('',*,*,#7841,.F.);
#10319=ORIENTED_EDGE('',*,*,#7842,.F.);
#10320=ORIENTED_EDGE('',*,*,#7843,.F.);
#10321=ORIENTED_EDGE('',*,*,#7842,.T.);
#10322=ORIENTED_EDGE('',*,*,#7844,.F.);
#10323=ORIENTED_EDGE('',*,*,#7845,.F.);
#10324=ORIENTED_EDGE('',*,*,#7846,.F.);
#10325=ORIENTED_EDGE('',*,*,#7845,.T.);
#10326=ORIENTED_EDGE('',*,*,#7847,.F.);
#10327=ORIENTED_EDGE('',*,*,#7848,.F.);
#10328=ORIENTED_EDGE('',*,*,#7849,.F.);
#10329=ORIENTED_EDGE('',*,*,#7848,.T.);
#10330=ORIENTED_EDGE('',*,*,#7850,.F.);
#10331=ORIENTED_EDGE('',*,*,#7851,.F.);
#10332=ORIENTED_EDGE('',*,*,#7852,.F.);
#10333=ORIENTED_EDGE('',*,*,#7851,.T.);
#10334=ORIENTED_EDGE('',*,*,#7853,.F.);
#10335=ORIENTED_EDGE('',*,*,#7854,.F.);
#10336=ORIENTED_EDGE('',*,*,#7855,.F.);
#10337=ORIENTED_EDGE('',*,*,#7854,.T.);
#10338=ORIENTED_EDGE('',*,*,#7856,.F.);
#10339=ORIENTED_EDGE('',*,*,#7857,.F.);
#10340=ORIENTED_EDGE('',*,*,#7858,.F.);
#10341=ORIENTED_EDGE('',*,*,#7857,.T.);
#10342=ORIENTED_EDGE('',*,*,#7859,.F.);
#10343=ORIENTED_EDGE('',*,*,#7860,.F.);
#10344=ORIENTED_EDGE('',*,*,#7861,.F.);
#10345=ORIENTED_EDGE('',*,*,#7860,.T.);
#10346=ORIENTED_EDGE('',*,*,#7862,.F.);
#10347=ORIENTED_EDGE('',*,*,#7863,.F.);
#10348=ORIENTED_EDGE('',*,*,#7864,.F.);
#10349=ORIENTED_EDGE('',*,*,#7863,.T.);
#10350=ORIENTED_EDGE('',*,*,#7865,.F.);
#10351=ORIENTED_EDGE('',*,*,#7866,.F.);
#10352=ORIENTED_EDGE('',*,*,#7867,.F.);
#10353=ORIENTED_EDGE('',*,*,#7866,.T.);
#10354=ORIENTED_EDGE('',*,*,#7868,.F.);
#10355=ORIENTED_EDGE('',*,*,#7869,.F.);
#10356=ORIENTED_EDGE('',*,*,#7870,.F.);
#10357=ORIENTED_EDGE('',*,*,#7869,.T.);
#10358=ORIENTED_EDGE('',*,*,#7871,.F.);
#10359=ORIENTED_EDGE('',*,*,#7872,.F.);
#10360=ORIENTED_EDGE('',*,*,#7873,.F.);
#10361=ORIENTED_EDGE('',*,*,#7872,.T.);
#10362=ORIENTED_EDGE('',*,*,#7874,.F.);
#10363=ORIENTED_EDGE('',*,*,#7875,.F.);
#10364=ORIENTED_EDGE('',*,*,#7876,.F.);
#10365=ORIENTED_EDGE('',*,*,#7875,.T.);
#10366=ORIENTED_EDGE('',*,*,#7877,.F.);
#10367=ORIENTED_EDGE('',*,*,#7878,.F.);
#10368=ORIENTED_EDGE('',*,*,#7879,.F.);
#10369=ORIENTED_EDGE('',*,*,#7878,.T.);
#10370=ORIENTED_EDGE('',*,*,#7880,.F.);
#10371=ORIENTED_EDGE('',*,*,#7881,.F.);
#10372=ORIENTED_EDGE('',*,*,#7882,.F.);
#10373=ORIENTED_EDGE('',*,*,#7881,.T.);
#10374=ORIENTED_EDGE('',*,*,#7883,.F.);
#10375=ORIENTED_EDGE('',*,*,#7394,.F.);
#10376=ORIENTED_EDGE('',*,*,#7883,.T.);
#10377=ORIENTED_EDGE('',*,*,#7880,.T.);
#10378=ORIENTED_EDGE('',*,*,#7877,.T.);
#10379=ORIENTED_EDGE('',*,*,#7874,.T.);
#10380=ORIENTED_EDGE('',*,*,#7871,.T.);
#10381=ORIENTED_EDGE('',*,*,#7868,.T.);
#10382=ORIENTED_EDGE('',*,*,#7865,.T.);
#10383=ORIENTED_EDGE('',*,*,#7862,.T.);
#10384=ORIENTED_EDGE('',*,*,#7859,.T.);
#10385=ORIENTED_EDGE('',*,*,#7856,.T.);
#10386=ORIENTED_EDGE('',*,*,#7853,.T.);
#10387=ORIENTED_EDGE('',*,*,#7850,.T.);
#10388=ORIENTED_EDGE('',*,*,#7847,.T.);
#10389=ORIENTED_EDGE('',*,*,#7844,.T.);
#10390=ORIENTED_EDGE('',*,*,#7841,.T.);
#10391=ORIENTED_EDGE('',*,*,#7838,.T.);
#10392=ORIENTED_EDGE('',*,*,#7835,.T.);
#10393=ORIENTED_EDGE('',*,*,#7832,.T.);
#10394=ORIENTED_EDGE('',*,*,#7829,.T.);
#10395=ORIENTED_EDGE('',*,*,#7826,.T.);
#10396=ORIENTED_EDGE('',*,*,#7823,.T.);
#10397=ORIENTED_EDGE('',*,*,#7820,.T.);
#10398=ORIENTED_EDGE('',*,*,#7817,.T.);
#10399=ORIENTED_EDGE('',*,*,#7814,.T.);
#10400=ORIENTED_EDGE('',*,*,#7811,.T.);
#10401=ORIENTED_EDGE('',*,*,#7808,.T.);
#10402=ORIENTED_EDGE('',*,*,#7805,.T.);
#10403=ORIENTED_EDGE('',*,*,#7802,.T.);
#10404=ORIENTED_EDGE('',*,*,#7799,.T.);
#10405=ORIENTED_EDGE('',*,*,#7796,.T.);
#10406=ORIENTED_EDGE('',*,*,#7793,.T.);
#10407=ORIENTED_EDGE('',*,*,#7790,.T.);
#10408=ORIENTED_EDGE('',*,*,#7787,.T.);
#10409=ORIENTED_EDGE('',*,*,#7784,.T.);
#10410=ORIENTED_EDGE('',*,*,#7781,.T.);
#10411=ORIENTED_EDGE('',*,*,#7778,.T.);
#10412=ORIENTED_EDGE('',*,*,#7775,.T.);
#10413=ORIENTED_EDGE('',*,*,#7772,.T.);
#10414=ORIENTED_EDGE('',*,*,#7769,.T.);
#10415=ORIENTED_EDGE('',*,*,#7766,.T.);
#10416=ORIENTED_EDGE('',*,*,#7763,.T.);
#10417=ORIENTED_EDGE('',*,*,#7760,.T.);
#10418=ORIENTED_EDGE('',*,*,#7757,.T.);
#10419=ORIENTED_EDGE('',*,*,#7754,.T.);
#10420=ORIENTED_EDGE('',*,*,#7751,.T.);
#10421=ORIENTED_EDGE('',*,*,#7748,.T.);
#10422=ORIENTED_EDGE('',*,*,#7745,.T.);
#10423=ORIENTED_EDGE('',*,*,#7742,.T.);
#10424=ORIENTED_EDGE('',*,*,#7739,.T.);
#10425=ORIENTED_EDGE('',*,*,#7736,.T.);
#10426=ORIENTED_EDGE('',*,*,#7733,.T.);
#10427=ORIENTED_EDGE('',*,*,#7730,.T.);
#10428=ORIENTED_EDGE('',*,*,#7727,.T.);
#10429=ORIENTED_EDGE('',*,*,#7724,.T.);
#10430=ORIENTED_EDGE('',*,*,#7721,.T.);
#10431=ORIENTED_EDGE('',*,*,#7718,.T.);
#10432=ORIENTED_EDGE('',*,*,#7715,.T.);
#10433=ORIENTED_EDGE('',*,*,#7712,.T.);
#10434=ORIENTED_EDGE('',*,*,#7709,.T.);
#10435=ORIENTED_EDGE('',*,*,#7706,.T.);
#10436=ORIENTED_EDGE('',*,*,#7703,.T.);
#10437=ORIENTED_EDGE('',*,*,#7700,.T.);
#10438=ORIENTED_EDGE('',*,*,#7697,.T.);
#10439=ORIENTED_EDGE('',*,*,#7694,.T.);
#10440=ORIENTED_EDGE('',*,*,#7691,.T.);
#10441=ORIENTED_EDGE('',*,*,#7688,.T.);
#10442=ORIENTED_EDGE('',*,*,#7685,.T.);
#10443=ORIENTED_EDGE('',*,*,#7682,.T.);
#10444=ORIENTED_EDGE('',*,*,#7679,.T.);
#10445=ORIENTED_EDGE('',*,*,#7676,.T.);
#10446=ORIENTED_EDGE('',*,*,#7673,.T.);
#10447=ORIENTED_EDGE('',*,*,#7670,.T.);
#10448=ORIENTED_EDGE('',*,*,#7667,.T.);
#10449=ORIENTED_EDGE('',*,*,#7664,.T.);
#10450=ORIENTED_EDGE('',*,*,#7661,.T.);
#10451=ORIENTED_EDGE('',*,*,#7658,.T.);
#10452=ORIENTED_EDGE('',*,*,#7655,.T.);
#10453=ORIENTED_EDGE('',*,*,#7652,.T.);
#10454=ORIENTED_EDGE('',*,*,#7649,.T.);
#10455=ORIENTED_EDGE('',*,*,#7646,.T.);
#10456=ORIENTED_EDGE('',*,*,#7643,.T.);
#10457=ORIENTED_EDGE('',*,*,#7640,.T.);
#10458=ORIENTED_EDGE('',*,*,#7637,.T.);
#10459=ORIENTED_EDGE('',*,*,#7634,.T.);
#10460=ORIENTED_EDGE('',*,*,#7631,.T.);
#10461=ORIENTED_EDGE('',*,*,#7628,.T.);
#10462=ORIENTED_EDGE('',*,*,#7625,.T.);
#10463=ORIENTED_EDGE('',*,*,#7622,.T.);
#10464=ORIENTED_EDGE('',*,*,#7619,.T.);
#10465=ORIENTED_EDGE('',*,*,#7616,.T.);
#10466=ORIENTED_EDGE('',*,*,#7613,.T.);
#10467=ORIENTED_EDGE('',*,*,#7610,.T.);
#10468=ORIENTED_EDGE('',*,*,#7607,.T.);
#10469=ORIENTED_EDGE('',*,*,#7604,.T.);
#10470=ORIENTED_EDGE('',*,*,#7601,.T.);
#10471=ORIENTED_EDGE('',*,*,#7598,.T.);
#10472=ORIENTED_EDGE('',*,*,#7595,.T.);
#10473=ORIENTED_EDGE('',*,*,#7592,.T.);
#10474=ORIENTED_EDGE('',*,*,#7589,.T.);
#10475=ORIENTED_EDGE('',*,*,#7586,.T.);
#10476=ORIENTED_EDGE('',*,*,#7583,.T.);
#10477=ORIENTED_EDGE('',*,*,#7580,.T.);
#10478=ORIENTED_EDGE('',*,*,#7577,.T.);
#10479=ORIENTED_EDGE('',*,*,#7574,.T.);
#10480=ORIENTED_EDGE('',*,*,#7571,.T.);
#10481=ORIENTED_EDGE('',*,*,#7568,.T.);
#10482=ORIENTED_EDGE('',*,*,#7565,.T.);
#10483=ORIENTED_EDGE('',*,*,#7562,.T.);
#10484=ORIENTED_EDGE('',*,*,#7559,.T.);
#10485=ORIENTED_EDGE('',*,*,#7556,.T.);
#10486=ORIENTED_EDGE('',*,*,#7553,.T.);
#10487=ORIENTED_EDGE('',*,*,#7550,.T.);
#10488=ORIENTED_EDGE('',*,*,#7547,.T.);
#10489=ORIENTED_EDGE('',*,*,#7544,.T.);
#10490=ORIENTED_EDGE('',*,*,#7541,.T.);
#10491=ORIENTED_EDGE('',*,*,#7538,.T.);
#10492=ORIENTED_EDGE('',*,*,#7535,.T.);
#10493=ORIENTED_EDGE('',*,*,#7532,.T.);
#10494=ORIENTED_EDGE('',*,*,#7529,.T.);
#10495=ORIENTED_EDGE('',*,*,#7526,.T.);
#10496=ORIENTED_EDGE('',*,*,#7523,.T.);
#10497=ORIENTED_EDGE('',*,*,#7520,.T.);
#10498=ORIENTED_EDGE('',*,*,#7517,.T.);
#10499=ORIENTED_EDGE('',*,*,#7514,.T.);
#10500=ORIENTED_EDGE('',*,*,#7511,.T.);
#10501=ORIENTED_EDGE('',*,*,#7508,.T.);
#10502=ORIENTED_EDGE('',*,*,#7505,.T.);
#10503=ORIENTED_EDGE('',*,*,#7502,.T.);
#10504=ORIENTED_EDGE('',*,*,#7499,.T.);
#10505=ORIENTED_EDGE('',*,*,#7496,.T.);
#10506=ORIENTED_EDGE('',*,*,#7493,.T.);
#10507=ORIENTED_EDGE('',*,*,#7490,.T.);
#10508=ORIENTED_EDGE('',*,*,#7487,.T.);
#10509=ORIENTED_EDGE('',*,*,#7484,.T.);
#10510=ORIENTED_EDGE('',*,*,#7481,.T.);
#10511=ORIENTED_EDGE('',*,*,#7478,.T.);
#10512=ORIENTED_EDGE('',*,*,#7475,.T.);
#10513=ORIENTED_EDGE('',*,*,#7472,.T.);
#10514=ORIENTED_EDGE('',*,*,#7469,.T.);
#10515=ORIENTED_EDGE('',*,*,#7466,.T.);
#10516=ORIENTED_EDGE('',*,*,#7463,.T.);
#10517=ORIENTED_EDGE('',*,*,#7460,.T.);
#10518=ORIENTED_EDGE('',*,*,#7457,.T.);
#10519=ORIENTED_EDGE('',*,*,#7454,.T.);
#10520=ORIENTED_EDGE('',*,*,#7451,.T.);
#10521=ORIENTED_EDGE('',*,*,#7448,.T.);
#10522=ORIENTED_EDGE('',*,*,#7445,.T.);
#10523=ORIENTED_EDGE('',*,*,#7442,.T.);
#10524=ORIENTED_EDGE('',*,*,#7439,.T.);
#10525=ORIENTED_EDGE('',*,*,#7436,.T.);
#10526=ORIENTED_EDGE('',*,*,#7433,.T.);
#10527=ORIENTED_EDGE('',*,*,#7430,.T.);
#10528=ORIENTED_EDGE('',*,*,#7427,.T.);
#10529=ORIENTED_EDGE('',*,*,#7424,.T.);
#10530=ORIENTED_EDGE('',*,*,#7421,.T.);
#10531=ORIENTED_EDGE('',*,*,#7418,.T.);
#10532=ORIENTED_EDGE('',*,*,#7415,.T.);
#10533=ORIENTED_EDGE('',*,*,#7412,.T.);
#10534=ORIENTED_EDGE('',*,*,#7409,.T.);
#10535=ORIENTED_EDGE('',*,*,#7406,.T.);
#10536=ORIENTED_EDGE('',*,*,#7403,.T.);
#10537=ORIENTED_EDGE('',*,*,#7398,.T.);
#10538=ORIENTED_EDGE('',*,*,#7390,.T.);
#10539=ORIENTED_EDGE('',*,*,#7395,.T.);
#10540=ORIENTED_EDGE('',*,*,#7882,.T.);
#10541=ORIENTED_EDGE('',*,*,#7393,.T.);
#10542=ORIENTED_EDGE('',*,*,#7386,.T.);
#10543=ORIENTED_EDGE('',*,*,#7400,.T.);
#10544=ORIENTED_EDGE('',*,*,#7402,.T.);
#10545=ORIENTED_EDGE('',*,*,#7405,.T.);
#10546=ORIENTED_EDGE('',*,*,#7408,.T.);
#10547=ORIENTED_EDGE('',*,*,#7411,.T.);
#10548=ORIENTED_EDGE('',*,*,#7414,.T.);
#10549=ORIENTED_EDGE('',*,*,#7417,.T.);
#10550=ORIENTED_EDGE('',*,*,#7420,.T.);
#10551=ORIENTED_EDGE('',*,*,#7423,.T.);
#10552=ORIENTED_EDGE('',*,*,#7426,.T.);
#10553=ORIENTED_EDGE('',*,*,#7429,.T.);
#10554=ORIENTED_EDGE('',*,*,#7432,.T.);
#10555=ORIENTED_EDGE('',*,*,#7435,.T.);
#10556=ORIENTED_EDGE('',*,*,#7438,.T.);
#10557=ORIENTED_EDGE('',*,*,#7441,.T.);
#10558=ORIENTED_EDGE('',*,*,#7444,.T.);
#10559=ORIENTED_EDGE('',*,*,#7447,.T.);
#10560=ORIENTED_EDGE('',*,*,#7450,.T.);
#10561=ORIENTED_EDGE('',*,*,#7453,.T.);
#10562=ORIENTED_EDGE('',*,*,#7456,.T.);
#10563=ORIENTED_EDGE('',*,*,#7459,.T.);
#10564=ORIENTED_EDGE('',*,*,#7462,.T.);
#10565=ORIENTED_EDGE('',*,*,#7465,.T.);
#10566=ORIENTED_EDGE('',*,*,#7468,.T.);
#10567=ORIENTED_EDGE('',*,*,#7471,.T.);
#10568=ORIENTED_EDGE('',*,*,#7474,.T.);
#10569=ORIENTED_EDGE('',*,*,#7477,.T.);
#10570=ORIENTED_EDGE('',*,*,#7480,.T.);
#10571=ORIENTED_EDGE('',*,*,#7483,.T.);
#10572=ORIENTED_EDGE('',*,*,#7486,.T.);
#10573=ORIENTED_EDGE('',*,*,#7489,.T.);
#10574=ORIENTED_EDGE('',*,*,#7492,.T.);
#10575=ORIENTED_EDGE('',*,*,#7495,.T.);
#10576=ORIENTED_EDGE('',*,*,#7498,.T.);
#10577=ORIENTED_EDGE('',*,*,#7501,.T.);
#10578=ORIENTED_EDGE('',*,*,#7504,.T.);
#10579=ORIENTED_EDGE('',*,*,#7507,.T.);
#10580=ORIENTED_EDGE('',*,*,#7510,.T.);
#10581=ORIENTED_EDGE('',*,*,#7513,.T.);
#10582=ORIENTED_EDGE('',*,*,#7516,.T.);
#10583=ORIENTED_EDGE('',*,*,#7519,.T.);
#10584=ORIENTED_EDGE('',*,*,#7522,.T.);
#10585=ORIENTED_EDGE('',*,*,#7525,.T.);
#10586=ORIENTED_EDGE('',*,*,#7528,.T.);
#10587=ORIENTED_EDGE('',*,*,#7531,.T.);
#10588=ORIENTED_EDGE('',*,*,#7534,.T.);
#10589=ORIENTED_EDGE('',*,*,#7537,.T.);
#10590=ORIENTED_EDGE('',*,*,#7540,.T.);
#10591=ORIENTED_EDGE('',*,*,#7543,.T.);
#10592=ORIENTED_EDGE('',*,*,#7546,.T.);
#10593=ORIENTED_EDGE('',*,*,#7549,.T.);
#10594=ORIENTED_EDGE('',*,*,#7552,.T.);
#10595=ORIENTED_EDGE('',*,*,#7555,.T.);
#10596=ORIENTED_EDGE('',*,*,#7558,.T.);
#10597=ORIENTED_EDGE('',*,*,#7561,.T.);
#10598=ORIENTED_EDGE('',*,*,#7564,.T.);
#10599=ORIENTED_EDGE('',*,*,#7567,.T.);
#10600=ORIENTED_EDGE('',*,*,#7570,.T.);
#10601=ORIENTED_EDGE('',*,*,#7573,.T.);
#10602=ORIENTED_EDGE('',*,*,#7576,.T.);
#10603=ORIENTED_EDGE('',*,*,#7579,.T.);
#10604=ORIENTED_EDGE('',*,*,#7582,.T.);
#10605=ORIENTED_EDGE('',*,*,#7585,.T.);
#10606=ORIENTED_EDGE('',*,*,#7588,.T.);
#10607=ORIENTED_EDGE('',*,*,#7591,.T.);
#10608=ORIENTED_EDGE('',*,*,#7594,.T.);
#10609=ORIENTED_EDGE('',*,*,#7597,.T.);
#10610=ORIENTED_EDGE('',*,*,#7600,.T.);
#10611=ORIENTED_EDGE('',*,*,#7603,.T.);
#10612=ORIENTED_EDGE('',*,*,#7606,.T.);
#10613=ORIENTED_EDGE('',*,*,#7609,.T.);
#10614=ORIENTED_EDGE('',*,*,#7612,.T.);
#10615=ORIENTED_EDGE('',*,*,#7615,.T.);
#10616=ORIENTED_EDGE('',*,*,#7618,.T.);
#10617=ORIENTED_EDGE('',*,*,#7621,.T.);
#10618=ORIENTED_EDGE('',*,*,#7624,.T.);
#10619=ORIENTED_EDGE('',*,*,#7627,.T.);
#10620=ORIENTED_EDGE('',*,*,#7630,.T.);
#10621=ORIENTED_EDGE('',*,*,#7633,.T.);
#10622=ORIENTED_EDGE('',*,*,#7636,.T.);
#10623=ORIENTED_EDGE('',*,*,#7639,.T.);
#10624=ORIENTED_EDGE('',*,*,#7642,.T.);
#10625=ORIENTED_EDGE('',*,*,#7645,.T.);
#10626=ORIENTED_EDGE('',*,*,#7648,.T.);
#10627=ORIENTED_EDGE('',*,*,#7651,.T.);
#10628=ORIENTED_EDGE('',*,*,#7654,.T.);
#10629=ORIENTED_EDGE('',*,*,#7657,.T.);
#10630=ORIENTED_EDGE('',*,*,#7660,.T.);
#10631=ORIENTED_EDGE('',*,*,#7663,.T.);
#10632=ORIENTED_EDGE('',*,*,#7666,.T.);
#10633=ORIENTED_EDGE('',*,*,#7669,.T.);
#10634=ORIENTED_EDGE('',*,*,#7672,.T.);
#10635=ORIENTED_EDGE('',*,*,#7675,.T.);
#10636=ORIENTED_EDGE('',*,*,#7678,.T.);
#10637=ORIENTED_EDGE('',*,*,#7681,.T.);
#10638=ORIENTED_EDGE('',*,*,#7684,.T.);
#10639=ORIENTED_EDGE('',*,*,#7687,.T.);
#10640=ORIENTED_EDGE('',*,*,#7690,.T.);
#10641=ORIENTED_EDGE('',*,*,#7693,.T.);
#10642=ORIENTED_EDGE('',*,*,#7696,.T.);
#10643=ORIENTED_EDGE('',*,*,#7699,.T.);
#10644=ORIENTED_EDGE('',*,*,#7702,.T.);
#10645=ORIENTED_EDGE('',*,*,#7705,.T.);
#10646=ORIENTED_EDGE('',*,*,#7708,.T.);
#10647=ORIENTED_EDGE('',*,*,#7711,.T.);
#10648=ORIENTED_EDGE('',*,*,#7714,.T.);
#10649=ORIENTED_EDGE('',*,*,#7717,.T.);
#10650=ORIENTED_EDGE('',*,*,#7720,.T.);
#10651=ORIENTED_EDGE('',*,*,#7723,.T.);
#10652=ORIENTED_EDGE('',*,*,#7726,.T.);
#10653=ORIENTED_EDGE('',*,*,#7729,.T.);
#10654=ORIENTED_EDGE('',*,*,#7732,.T.);
#10655=ORIENTED_EDGE('',*,*,#7735,.T.);
#10656=ORIENTED_EDGE('',*,*,#7738,.T.);
#10657=ORIENTED_EDGE('',*,*,#7741,.T.);
#10658=ORIENTED_EDGE('',*,*,#7744,.T.);
#10659=ORIENTED_EDGE('',*,*,#7747,.T.);
#10660=ORIENTED_EDGE('',*,*,#7750,.T.);
#10661=ORIENTED_EDGE('',*,*,#7753,.T.);
#10662=ORIENTED_EDGE('',*,*,#7756,.T.);
#10663=ORIENTED_EDGE('',*,*,#7759,.T.);
#10664=ORIENTED_EDGE('',*,*,#7762,.T.);
#10665=ORIENTED_EDGE('',*,*,#7765,.T.);
#10666=ORIENTED_EDGE('',*,*,#7768,.T.);
#10667=ORIENTED_EDGE('',*,*,#7771,.T.);
#10668=ORIENTED_EDGE('',*,*,#7774,.T.);
#10669=ORIENTED_EDGE('',*,*,#7777,.T.);
#10670=ORIENTED_EDGE('',*,*,#7780,.T.);
#10671=ORIENTED_EDGE('',*,*,#7783,.T.);
#10672=ORIENTED_EDGE('',*,*,#7786,.T.);
#10673=ORIENTED_EDGE('',*,*,#7789,.T.);
#10674=ORIENTED_EDGE('',*,*,#7792,.T.);
#10675=ORIENTED_EDGE('',*,*,#7795,.T.);
#10676=ORIENTED_EDGE('',*,*,#7798,.T.);
#10677=ORIENTED_EDGE('',*,*,#7801,.T.);
#10678=ORIENTED_EDGE('',*,*,#7804,.T.);
#10679=ORIENTED_EDGE('',*,*,#7807,.T.);
#10680=ORIENTED_EDGE('',*,*,#7810,.T.);
#10681=ORIENTED_EDGE('',*,*,#7813,.T.);
#10682=ORIENTED_EDGE('',*,*,#7816,.T.);
#10683=ORIENTED_EDGE('',*,*,#7819,.T.);
#10684=ORIENTED_EDGE('',*,*,#7822,.T.);
#10685=ORIENTED_EDGE('',*,*,#7825,.T.);
#10686=ORIENTED_EDGE('',*,*,#7828,.T.);
#10687=ORIENTED_EDGE('',*,*,#7831,.T.);
#10688=ORIENTED_EDGE('',*,*,#7834,.T.);
#10689=ORIENTED_EDGE('',*,*,#7837,.T.);
#10690=ORIENTED_EDGE('',*,*,#7840,.T.);
#10691=ORIENTED_EDGE('',*,*,#7843,.T.);
#10692=ORIENTED_EDGE('',*,*,#7846,.T.);
#10693=ORIENTED_EDGE('',*,*,#7849,.T.);
#10694=ORIENTED_EDGE('',*,*,#7852,.T.);
#10695=ORIENTED_EDGE('',*,*,#7855,.T.);
#10696=ORIENTED_EDGE('',*,*,#7858,.T.);
#10697=ORIENTED_EDGE('',*,*,#7861,.T.);
#10698=ORIENTED_EDGE('',*,*,#7864,.T.);
#10699=ORIENTED_EDGE('',*,*,#7867,.T.);
#10700=ORIENTED_EDGE('',*,*,#7870,.T.);
#10701=ORIENTED_EDGE('',*,*,#7873,.T.);
#10702=ORIENTED_EDGE('',*,*,#7876,.T.);
#10703=ORIENTED_EDGE('',*,*,#7879,.T.);
#10704=ORIENTED_EDGE('',*,*,#7884,.F.);
#10705=ORIENTED_EDGE('',*,*,#7885,.T.);
#10706=ORIENTED_EDGE('',*,*,#7401,.T.);
#10707=ORIENTED_EDGE('',*,*,#7384,.T.);
#10708=ORIENTED_EDGE('',*,*,#7392,.T.);
#10709=ORIENTED_EDGE('',*,*,#7886,.T.);
#10710=ORIENTED_EDGE('',*,*,#7887,.T.);
#10711=ORIENTED_EDGE('',*,*,#7886,.F.);
#10712=ORIENTED_EDGE('',*,*,#7396,.T.);
#10713=ORIENTED_EDGE('',*,*,#7388,.T.);
#10714=ORIENTED_EDGE('',*,*,#7397,.T.);
#10715=ORIENTED_EDGE('',*,*,#7885,.F.);
#10716=ORIENTED_EDGE('',*,*,#7884,.T.);
#10717=ORIENTED_EDGE('',*,*,#7887,.F.);
#10718=ORIENTED_EDGE('',*,*,#7381,.T.);
#10719=ORIENTED_EDGE('',*,*,#7888,.F.);
#10720=ORIENTED_EDGE('',*,*,#7889,.T.);
#10721=ORIENTED_EDGE('',*,*,#7890,.F.);
#10722=ORIENTED_EDGE('',*,*,#7891,.F.);
#10723=ORIENTED_EDGE('',*,*,#7892,.F.);
#10724=ORIENTED_EDGE('',*,*,#7893,.T.);
#10725=ORIENTED_EDGE('',*,*,#7894,.F.);
#10726=ORIENTED_EDGE('',*,*,#7895,.F.);
#10727=ORIENTED_EDGE('',*,*,#7893,.F.);
#10728=ORIENTED_EDGE('',*,*,#7896,.F.);
#10729=ORIENTED_EDGE('',*,*,#7889,.F.);
#10730=ORIENTED_EDGE('',*,*,#7897,.F.);
#10731=ORIENTED_EDGE('',*,*,#7891,.T.);
#10732=ORIENTED_EDGE('',*,*,#7898,.F.);
#10733=ORIENTED_EDGE('',*,*,#7899,.T.);
#10734=ORIENTED_EDGE('',*,*,#7900,.F.);
#10735=ORIENTED_EDGE('',*,*,#7899,.F.);
#10736=ORIENTED_EDGE('',*,*,#7896,.T.);
#10737=ORIENTED_EDGE('',*,*,#7892,.T.);
#10738=ORIENTED_EDGE('',*,*,#7897,.T.);
#10739=ORIENTED_EDGE('',*,*,#7890,.T.);
#10740=ORIENTED_EDGE('',*,*,#7888,.T.);
#10741=ORIENTED_EDGE('',*,*,#7901,.F.);
#10742=ORIENTED_EDGE('',*,*,#7902,.T.);
#10743=ORIENTED_EDGE('',*,*,#7903,.F.);
#10744=ORIENTED_EDGE('',*,*,#7902,.F.);
#10745=ORIENTED_EDGE('',*,*,#7901,.T.);
#10746=ORIENTED_EDGE('',*,*,#7900,.T.);
#10747=ORIENTED_EDGE('',*,*,#7904,.F.);
#10748=ORIENTED_EDGE('',*,*,#7905,.T.);
#10749=ORIENTED_EDGE('',*,*,#7906,.T.);
#10750=ORIENTED_EDGE('',*,*,#7905,.F.);
#10751=ORIENTED_EDGE('',*,*,#7894,.T.);
#10752=ORIENTED_EDGE('',*,*,#7895,.T.);
#10753=ORIENTED_EDGE('',*,*,#7904,.T.);
#10754=ORIENTED_EDGE('',*,*,#7903,.T.);
#10755=ORIENTED_EDGE('',*,*,#7906,.F.);
#10756=ORIENTED_EDGE('',*,*,#7898,.T.);
#10757=ORIENTED_EDGE('',*,*,#7907,.F.);
#10758=ORIENTED_EDGE('',*,*,#7908,.T.);
#10759=ORIENTED_EDGE('',*,*,#7909,.T.);
#10760=ORIENTED_EDGE('',*,*,#7908,.F.);
#10761=ORIENTED_EDGE('',*,*,#7907,.T.);
#10762=ORIENTED_EDGE('',*,*,#7909,.F.);
#10763=ORIENTED_EDGE('',*,*,#7910,.F.);
#10764=ORIENTED_EDGE('',*,*,#7911,.T.);
#10765=ORIENTED_EDGE('',*,*,#7912,.T.);
#10766=ORIENTED_EDGE('',*,*,#7911,.F.);
#10767=ORIENTED_EDGE('',*,*,#7910,.T.);
#10768=ORIENTED_EDGE('',*,*,#7912,.F.);
#10769=ORIENTED_EDGE('',*,*,#7913,.F.);
#10770=ORIENTED_EDGE('',*,*,#7914,.F.);
#10771=ORIENTED_EDGE('',*,*,#7915,.T.);
#10772=ORIENTED_EDGE('',*,*,#7916,.F.);
#10773=ORIENTED_EDGE('',*,*,#7917,.F.);
#10774=ORIENTED_EDGE('',*,*,#7915,.F.);
#10775=ORIENTED_EDGE('',*,*,#7918,.F.);
#10776=ORIENTED_EDGE('',*,*,#7919,.T.);
#10777=ORIENTED_EDGE('',*,*,#7920,.F.);
#10778=ORIENTED_EDGE('',*,*,#7921,.F.);
#10779=ORIENTED_EDGE('',*,*,#7922,.F.);
#10780=ORIENTED_EDGE('',*,*,#7923,.T.);
#10781=ORIENTED_EDGE('',*,*,#7924,.F.);
#10782=ORIENTED_EDGE('',*,*,#7925,.F.);
#10783=ORIENTED_EDGE('',*,*,#7926,.F.);
#10784=ORIENTED_EDGE('',*,*,#7927,.F.);
#10785=ORIENTED_EDGE('',*,*,#7928,.F.);
#10786=ORIENTED_EDGE('',*,*,#7919,.F.);
#10787=ORIENTED_EDGE('',*,*,#7929,.F.);
#10788=ORIENTED_EDGE('',*,*,#7930,.F.);
#10789=ORIENTED_EDGE('',*,*,#7931,.F.);
#10790=ORIENTED_EDGE('',*,*,#7923,.F.);
#10791=ORIENTED_EDGE('',*,*,#7920,.T.);
#10792=ORIENTED_EDGE('',*,*,#7928,.T.);
#10793=ORIENTED_EDGE('',*,*,#7932,.T.);
#10794=ORIENTED_EDGE('',*,*,#7924,.T.);
#10795=ORIENTED_EDGE('',*,*,#7931,.T.);
#10796=ORIENTED_EDGE('',*,*,#7933,.T.);
#10797=ORIENTED_EDGE('',*,*,#7921,.T.);
#10798=ORIENTED_EDGE('',*,*,#7933,.F.);
#10799=ORIENTED_EDGE('',*,*,#7930,.T.);
#10800=ORIENTED_EDGE('',*,*,#7934,.T.);
#10801=ORIENTED_EDGE('',*,*,#7916,.T.);
#10802=ORIENTED_EDGE('',*,*,#7917,.T.);
#10803=ORIENTED_EDGE('',*,*,#7927,.T.);
#10804=ORIENTED_EDGE('',*,*,#7935,.T.);
#10805=ORIENTED_EDGE('',*,*,#7925,.T.);
#10806=ORIENTED_EDGE('',*,*,#7932,.F.);
#10807=ORIENTED_EDGE('',*,*,#7913,.T.);
#10808=ORIENTED_EDGE('',*,*,#7914,.T.);
#10809=ORIENTED_EDGE('',*,*,#7918,.T.);
#10810=ORIENTED_EDGE('',*,*,#7934,.F.);
#10811=ORIENTED_EDGE('',*,*,#7929,.T.);
#10812=ORIENTED_EDGE('',*,*,#7922,.T.);
#10813=ORIENTED_EDGE('',*,*,#7935,.F.);
#10814=ORIENTED_EDGE('',*,*,#7926,.T.);
#10815=ORIENTED_EDGE('',*,*,#7936,.F.);
#10816=ORIENTED_EDGE('',*,*,#7937,.T.);
#10817=ORIENTED_EDGE('',*,*,#7938,.T.);
#10818=ORIENTED_EDGE('',*,*,#7939,.F.);
#10819=ORIENTED_EDGE('',*,*,#7940,.F.);
#10820=ORIENTED_EDGE('',*,*,#7941,.T.);
#10821=ORIENTED_EDGE('',*,*,#7942,.T.);
#10822=ORIENTED_EDGE('',*,*,#7937,.F.);
#10823=ORIENTED_EDGE('',*,*,#7943,.F.);
#10824=ORIENTED_EDGE('',*,*,#7944,.T.);
#10825=ORIENTED_EDGE('',*,*,#7945,.T.);
#10826=ORIENTED_EDGE('',*,*,#7941,.F.);
#10827=ORIENTED_EDGE('',*,*,#7946,.F.);
#10828=ORIENTED_EDGE('',*,*,#7947,.T.);
#10829=ORIENTED_EDGE('',*,*,#7948,.T.);
#10830=ORIENTED_EDGE('',*,*,#7944,.F.);
#10831=ORIENTED_EDGE('',*,*,#7949,.F.);
#10832=ORIENTED_EDGE('',*,*,#7950,.T.);
#10833=ORIENTED_EDGE('',*,*,#7951,.T.);
#10834=ORIENTED_EDGE('',*,*,#7947,.F.);
#10835=ORIENTED_EDGE('',*,*,#7952,.F.);
#10836=ORIENTED_EDGE('',*,*,#7939,.T.);
#10837=ORIENTED_EDGE('',*,*,#7953,.T.);
#10838=ORIENTED_EDGE('',*,*,#7950,.F.);
#10839=ORIENTED_EDGE('',*,*,#7953,.F.);
#10840=ORIENTED_EDGE('',*,*,#7938,.F.);
#10841=ORIENTED_EDGE('',*,*,#7942,.F.);
#10842=ORIENTED_EDGE('',*,*,#7945,.F.);
#10843=ORIENTED_EDGE('',*,*,#7948,.F.);
#10844=ORIENTED_EDGE('',*,*,#7951,.F.);
#10845=ORIENTED_EDGE('',*,*,#7954,.F.);
#10846=ORIENTED_EDGE('',*,*,#7936,.T.);
#10847=ORIENTED_EDGE('',*,*,#7952,.T.);
#10848=ORIENTED_EDGE('',*,*,#7949,.T.);
#10849=ORIENTED_EDGE('',*,*,#7946,.T.);
#10850=ORIENTED_EDGE('',*,*,#7943,.T.);
#10851=ORIENTED_EDGE('',*,*,#7940,.T.);
#10852=ORIENTED_EDGE('',*,*,#7955,.F.);
#10853=ORIENTED_EDGE('',*,*,#7956,.T.);
#10854=ORIENTED_EDGE('',*,*,#7954,.T.);
#10855=ORIENTED_EDGE('',*,*,#7956,.F.);
#10856=ORIENTED_EDGE('',*,*,#7957,.F.);
#10857=ORIENTED_EDGE('',*,*,#7958,.T.);
#10858=ORIENTED_EDGE('',*,*,#7955,.T.);
#10859=ORIENTED_EDGE('',*,*,#7958,.F.);
#10860=ORIENTED_EDGE('',*,*,#7959,.F.);
#10861=ORIENTED_EDGE('',*,*,#7960,.T.);
#10862=ORIENTED_EDGE('',*,*,#7957,.T.);
#10863=ORIENTED_EDGE('',*,*,#7960,.F.);
#10864=ORIENTED_EDGE('',*,*,#7959,.T.);
#10865=ORIENTED_EDGE('',*,*,#7961,.F.);
#10866=ORIENTED_EDGE('',*,*,#7962,.T.);
#10867=ORIENTED_EDGE('',*,*,#7963,.F.);
#10868=ORIENTED_EDGE('',*,*,#7962,.F.);
#10869=ORIENTED_EDGE('',*,*,#7961,.T.);
#10870=ORIENTED_EDGE('',*,*,#7964,.F.);
#10871=ORIENTED_EDGE('',*,*,#7965,.T.);
#10872=ORIENTED_EDGE('',*,*,#7966,.T.);
#10873=ORIENTED_EDGE('',*,*,#7965,.F.);
#10874=ORIENTED_EDGE('',*,*,#7966,.F.);
#10875=ORIENTED_EDGE('',*,*,#7967,.F.);
#10876=ORIENTED_EDGE('',*,*,#7968,.T.);
#10877=ORIENTED_EDGE('',*,*,#7969,.F.);
#10878=ORIENTED_EDGE('',*,*,#7970,.T.);
#10879=ORIENTED_EDGE('',*,*,#7971,.F.);
#10880=ORIENTED_EDGE('',*,*,#7970,.F.);
#10881=ORIENTED_EDGE('',*,*,#7972,.F.);
#10882=ORIENTED_EDGE('',*,*,#7973,.F.);
#10883=ORIENTED_EDGE('',*,*,#7972,.T.);
#10884=ORIENTED_EDGE('',*,*,#7969,.T.);
#10885=ORIENTED_EDGE('',*,*,#7974,.T.);
#10886=ORIENTED_EDGE('',*,*,#7975,.F.);
#10887=ORIENTED_EDGE('',*,*,#7976,.F.);
#10888=ORIENTED_EDGE('',*,*,#7973,.T.);
#10889=ORIENTED_EDGE('',*,*,#7975,.T.);
#10890=ORIENTED_EDGE('',*,*,#7977,.T.);
#10891=ORIENTED_EDGE('',*,*,#7978,.F.);
#10892=ORIENTED_EDGE('',*,*,#7977,.F.);
#10893=ORIENTED_EDGE('',*,*,#7974,.F.);
#10894=ORIENTED_EDGE('',*,*,#7968,.F.);
#10895=ORIENTED_EDGE('',*,*,#7979,.F.);
#10896=ORIENTED_EDGE('',*,*,#7980,.T.);
#10897=ORIENTED_EDGE('',*,*,#7981,.F.);
#10898=ORIENTED_EDGE('',*,*,#7982,.T.);
#10899=ORIENTED_EDGE('',*,*,#7983,.F.);
#10900=ORIENTED_EDGE('',*,*,#7982,.F.);
#10901=ORIENTED_EDGE('',*,*,#7984,.F.);
#10902=ORIENTED_EDGE('',*,*,#7985,.F.);
#10903=ORIENTED_EDGE('',*,*,#7984,.T.);
#10904=ORIENTED_EDGE('',*,*,#7981,.T.);
#10905=ORIENTED_EDGE('',*,*,#7986,.T.);
#10906=ORIENTED_EDGE('',*,*,#7987,.F.);
#10907=ORIENTED_EDGE('',*,*,#7988,.F.);
#10908=ORIENTED_EDGE('',*,*,#7985,.T.);
#10909=ORIENTED_EDGE('',*,*,#7987,.T.);
#10910=ORIENTED_EDGE('',*,*,#7989,.T.);
#10911=ORIENTED_EDGE('',*,*,#7990,.F.);
#10912=ORIENTED_EDGE('',*,*,#7989,.F.);
#10913=ORIENTED_EDGE('',*,*,#7986,.F.);
#10914=ORIENTED_EDGE('',*,*,#7980,.F.);
#10915=ORIENTED_EDGE('',*,*,#7991,.F.);
#10916=ORIENTED_EDGE('',*,*,#7992,.T.);
#10917=ORIENTED_EDGE('',*,*,#7993,.T.);
#10918=ORIENTED_EDGE('',*,*,#7992,.F.);
#10919=ORIENTED_EDGE('',*,*,#7976,.T.);
#10920=ORIENTED_EDGE('',*,*,#7978,.T.);
#10921=ORIENTED_EDGE('',*,*,#7967,.T.);
#10922=ORIENTED_EDGE('',*,*,#7971,.T.);
#10923=ORIENTED_EDGE('',*,*,#7988,.T.);
#10924=ORIENTED_EDGE('',*,*,#7990,.T.);
#10925=ORIENTED_EDGE('',*,*,#7979,.T.);
#10926=ORIENTED_EDGE('',*,*,#7983,.T.);
#10927=ORIENTED_EDGE('',*,*,#7991,.T.);
#10928=ORIENTED_EDGE('',*,*,#7963,.T.);
#10929=ORIENTED_EDGE('',*,*,#7993,.F.);
#10930=ORIENTED_EDGE('',*,*,#7964,.T.);
#10931=ORIENTED_EDGE('',*,*,#7994,.F.);
#10932=ORIENTED_EDGE('',*,*,#7995,.T.);
#10933=ORIENTED_EDGE('',*,*,#7996,.T.);
#10934=ORIENTED_EDGE('',*,*,#7995,.F.);
#10935=ORIENTED_EDGE('',*,*,#7997,.F.);
#10936=ORIENTED_EDGE('',*,*,#7998,.T.);
#10937=ORIENTED_EDGE('',*,*,#7999,.T.);
#10938=ORIENTED_EDGE('',*,*,#7998,.F.);
#10939=ORIENTED_EDGE('',*,*,#7997,.T.);
#10940=ORIENTED_EDGE('',*,*,#7994,.T.);
#10941=ORIENTED_EDGE('',*,*,#7999,.F.);
#10942=ORIENTED_EDGE('',*,*,#7996,.F.);
#10943=ORIENTED_EDGE('',*,*,#8000,.F.);
#10944=ORIENTED_EDGE('',*,*,#8001,.T.);
#10945=ORIENTED_EDGE('',*,*,#8002,.T.);
#10946=ORIENTED_EDGE('',*,*,#8001,.F.);
#10947=ORIENTED_EDGE('',*,*,#8003,.F.);
#10948=ORIENTED_EDGE('',*,*,#8004,.T.);
#10949=ORIENTED_EDGE('',*,*,#8005,.T.);
#10950=ORIENTED_EDGE('',*,*,#8004,.F.);
#10951=ORIENTED_EDGE('',*,*,#8003,.T.);
#10952=ORIENTED_EDGE('',*,*,#8000,.T.);
#10953=ORIENTED_EDGE('',*,*,#8005,.F.);
#10954=ORIENTED_EDGE('',*,*,#8002,.F.);
#10955=ORIENTED_EDGE('',*,*,#8006,.F.);
#10956=ORIENTED_EDGE('',*,*,#8007,.T.);
#10957=ORIENTED_EDGE('',*,*,#8008,.T.);
#10958=ORIENTED_EDGE('',*,*,#8007,.F.);
#10959=ORIENTED_EDGE('',*,*,#8009,.F.);
#10960=ORIENTED_EDGE('',*,*,#8010,.T.);
#10961=ORIENTED_EDGE('',*,*,#8011,.T.);
#10962=ORIENTED_EDGE('',*,*,#8010,.F.);
#10963=ORIENTED_EDGE('',*,*,#8009,.T.);
#10964=ORIENTED_EDGE('',*,*,#8006,.T.);
#10965=ORIENTED_EDGE('',*,*,#8011,.F.);
#10966=ORIENTED_EDGE('',*,*,#8008,.F.);
#10967=ORIENTED_EDGE('',*,*,#8012,.F.);
#10968=ORIENTED_EDGE('',*,*,#8013,.T.);
#10969=ORIENTED_EDGE('',*,*,#8014,.T.);
#10970=ORIENTED_EDGE('',*,*,#8013,.F.);
#10971=ORIENTED_EDGE('',*,*,#8015,.F.);
#10972=ORIENTED_EDGE('',*,*,#8016,.T.);
#10973=ORIENTED_EDGE('',*,*,#8017,.T.);
#10974=ORIENTED_EDGE('',*,*,#8016,.F.);
#10975=ORIENTED_EDGE('',*,*,#8015,.T.);
#10976=ORIENTED_EDGE('',*,*,#8012,.T.);
#10977=ORIENTED_EDGE('',*,*,#8017,.F.);
#10978=ORIENTED_EDGE('',*,*,#8014,.F.);
#10979=ORIENTED_EDGE('',*,*,#8018,.T.);
#10980=ORIENTED_EDGE('',*,*,#8019,.T.);
#10981=ORIENTED_EDGE('',*,*,#8020,.F.);
#10982=ORIENTED_EDGE('',*,*,#8021,.F.);
#10983=ORIENTED_EDGE('',*,*,#8022,.T.);
#10984=ORIENTED_EDGE('',*,*,#8021,.T.);
#10985=ORIENTED_EDGE('',*,*,#8023,.F.);
#10986=ORIENTED_EDGE('',*,*,#8024,.F.);
#10987=ORIENTED_EDGE('',*,*,#8025,.T.);
#10988=ORIENTED_EDGE('',*,*,#8024,.T.);
#10989=ORIENTED_EDGE('',*,*,#8026,.F.);
#10990=ORIENTED_EDGE('',*,*,#8027,.F.);
#10991=ORIENTED_EDGE('',*,*,#8028,.T.);
#10992=ORIENTED_EDGE('',*,*,#8027,.T.);
#10993=ORIENTED_EDGE('',*,*,#8029,.F.);
#10994=ORIENTED_EDGE('',*,*,#8019,.F.);
#10995=ORIENTED_EDGE('',*,*,#8029,.T.);
#10996=ORIENTED_EDGE('',*,*,#8026,.T.);
#10997=ORIENTED_EDGE('',*,*,#8023,.T.);
#10998=ORIENTED_EDGE('',*,*,#8020,.T.);
#10999=ORIENTED_EDGE('',*,*,#8028,.F.);
#11000=ORIENTED_EDGE('',*,*,#8018,.F.);
#11001=ORIENTED_EDGE('',*,*,#8022,.F.);
#11002=ORIENTED_EDGE('',*,*,#8025,.F.);
#11003=ORIENTED_EDGE('',*,*,#8030,.T.);
#11004=ORIENTED_EDGE('',*,*,#8031,.T.);
#11005=ORIENTED_EDGE('',*,*,#8032,.F.);
#11006=ORIENTED_EDGE('',*,*,#8033,.F.);
#11007=ORIENTED_EDGE('',*,*,#8034,.T.);
#11008=ORIENTED_EDGE('',*,*,#8033,.T.);
#11009=ORIENTED_EDGE('',*,*,#8035,.F.);
#11010=ORIENTED_EDGE('',*,*,#8036,.F.);
#11011=ORIENTED_EDGE('',*,*,#8037,.T.);
#11012=ORIENTED_EDGE('',*,*,#8036,.T.);
#11013=ORIENTED_EDGE('',*,*,#8038,.F.);
#11014=ORIENTED_EDGE('',*,*,#8039,.F.);
#11015=ORIENTED_EDGE('',*,*,#8040,.T.);
#11016=ORIENTED_EDGE('',*,*,#8039,.T.);
#11017=ORIENTED_EDGE('',*,*,#8041,.F.);
#11018=ORIENTED_EDGE('',*,*,#8031,.F.);
#11019=ORIENTED_EDGE('',*,*,#8041,.T.);
#11020=ORIENTED_EDGE('',*,*,#8038,.T.);
#11021=ORIENTED_EDGE('',*,*,#8035,.T.);
#11022=ORIENTED_EDGE('',*,*,#8032,.T.);
#11023=ORIENTED_EDGE('',*,*,#8040,.F.);
#11024=ORIENTED_EDGE('',*,*,#8030,.F.);
#11025=ORIENTED_EDGE('',*,*,#8034,.F.);
#11026=ORIENTED_EDGE('',*,*,#8037,.F.);
#11027=ORIENTED_EDGE('',*,*,#8042,.F.);
#11028=ORIENTED_EDGE('',*,*,#8043,.T.);
#11029=ORIENTED_EDGE('',*,*,#8044,.F.);
#11030=ORIENTED_EDGE('',*,*,#8043,.F.);
#11031=ORIENTED_EDGE('',*,*,#8045,.F.);
#11032=ORIENTED_EDGE('',*,*,#8046,.T.);
#11033=ORIENTED_EDGE('',*,*,#8047,.F.);
#11034=ORIENTED_EDGE('',*,*,#8048,.F.);
#11035=ORIENTED_EDGE('',*,*,#8049,.F.);
#11036=ORIENTED_EDGE('',*,*,#8050,.T.);
#11037=ORIENTED_EDGE('',*,*,#8051,.F.);
#11038=ORIENTED_EDGE('',*,*,#8046,.F.);
#11039=ORIENTED_EDGE('',*,*,#8052,.F.);
#11040=ORIENTED_EDGE('',*,*,#8053,.F.);
#11041=ORIENTED_EDGE('',*,*,#8054,.F.);
#11042=ORIENTED_EDGE('',*,*,#8050,.F.);
#11043=ORIENTED_EDGE('',*,*,#8055,.T.);
#11044=ORIENTED_EDGE('',*,*,#8047,.T.);
#11045=ORIENTED_EDGE('',*,*,#8051,.T.);
#11046=ORIENTED_EDGE('',*,*,#8054,.T.);
#11047=ORIENTED_EDGE('',*,*,#8056,.T.);
#11048=ORIENTED_EDGE('',*,*,#8048,.T.);
#11049=ORIENTED_EDGE('',*,*,#8056,.F.);
#11050=ORIENTED_EDGE('',*,*,#8053,.T.);
#11051=ORIENTED_EDGE('',*,*,#8057,.T.);
#11052=ORIENTED_EDGE('',*,*,#8058,.F.);
#11053=ORIENTED_EDGE('',*,*,#8059,.F.);
#11054=ORIENTED_EDGE('',*,*,#8060,.F.);
#11055=ORIENTED_EDGE('',*,*,#8061,.T.);
#11056=ORIENTED_EDGE('',*,*,#8058,.T.);
#11057=ORIENTED_EDGE('',*,*,#8062,.F.);
#11058=ORIENTED_EDGE('',*,*,#8063,.F.);
#11059=ORIENTED_EDGE('',*,*,#8064,.F.);
#11060=ORIENTED_EDGE('',*,*,#8061,.F.);
#11061=ORIENTED_EDGE('',*,*,#8065,.T.);
#11062=ORIENTED_EDGE('',*,*,#8066,.F.);
#11063=ORIENTED_EDGE('',*,*,#8062,.T.);
#11064=ORIENTED_EDGE('',*,*,#8042,.T.);
#11065=ORIENTED_EDGE('',*,*,#8060,.T.);
#11066=ORIENTED_EDGE('',*,*,#8067,.F.);
#11067=ORIENTED_EDGE('',*,*,#8068,.F.);
#11068=ORIENTED_EDGE('',*,*,#8065,.F.);
#11069=ORIENTED_EDGE('',*,*,#8064,.T.);
#11070=ORIENTED_EDGE('',*,*,#8069,.F.);
#11071=ORIENTED_EDGE('',*,*,#8067,.T.);
#11072=ORIENTED_EDGE('',*,*,#8059,.T.);
#11073=ORIENTED_EDGE('',*,*,#8044,.T.);
#11074=ORIENTED_EDGE('',*,*,#8055,.F.);
#11075=ORIENTED_EDGE('',*,*,#8070,.T.);
#11076=ORIENTED_EDGE('',*,*,#8071,.T.);
#11077=ORIENTED_EDGE('',*,*,#8070,.F.);
#11078=ORIENTED_EDGE('',*,*,#8063,.T.);
#11079=ORIENTED_EDGE('',*,*,#8066,.T.);
#11080=ORIENTED_EDGE('',*,*,#8068,.T.);
#11081=ORIENTED_EDGE('',*,*,#8069,.T.);
#11082=ORIENTED_EDGE('',*,*,#8071,.F.);
#11083=ORIENTED_EDGE('',*,*,#8045,.T.);
#11084=ORIENTED_EDGE('',*,*,#8057,.F.);
#11085=ORIENTED_EDGE('',*,*,#8052,.T.);
#11086=ORIENTED_EDGE('',*,*,#8049,.T.);
#11087=ORIENTED_EDGE('',*,*,#8072,.F.);
#11088=ORIENTED_EDGE('',*,*,#8073,.T.);
#11089=ORIENTED_EDGE('',*,*,#8074,.T.);
#11090=ORIENTED_EDGE('',*,*,#8073,.F.);
#11091=ORIENTED_EDGE('',*,*,#8075,.F.);
#11092=ORIENTED_EDGE('',*,*,#8076,.T.);
#11093=ORIENTED_EDGE('',*,*,#8077,.T.);
#11094=ORIENTED_EDGE('',*,*,#8076,.F.);
#11095=ORIENTED_EDGE('',*,*,#8075,.T.);
#11096=ORIENTED_EDGE('',*,*,#8072,.T.);
#11097=ORIENTED_EDGE('',*,*,#8077,.F.);
#11098=ORIENTED_EDGE('',*,*,#8074,.F.);
#11099=ORIENTED_EDGE('',*,*,#8078,.F.);
#11100=ORIENTED_EDGE('',*,*,#8079,.T.);
#11101=ORIENTED_EDGE('',*,*,#8080,.T.);
#11102=ORIENTED_EDGE('',*,*,#8079,.F.);
#11103=ORIENTED_EDGE('',*,*,#8081,.F.);
#11104=ORIENTED_EDGE('',*,*,#8082,.T.);
#11105=ORIENTED_EDGE('',*,*,#8083,.T.);
#11106=ORIENTED_EDGE('',*,*,#8082,.F.);
#11107=ORIENTED_EDGE('',*,*,#8081,.T.);
#11108=ORIENTED_EDGE('',*,*,#8078,.T.);
#11109=ORIENTED_EDGE('',*,*,#8083,.F.);
#11110=ORIENTED_EDGE('',*,*,#8080,.F.);
#11111=ORIENTED_EDGE('',*,*,#8084,.F.);
#11112=ORIENTED_EDGE('',*,*,#8085,.T.);
#11113=ORIENTED_EDGE('',*,*,#8086,.T.);
#11114=ORIENTED_EDGE('',*,*,#8085,.F.);
#11115=ORIENTED_EDGE('',*,*,#8087,.F.);
#11116=ORIENTED_EDGE('',*,*,#8088,.T.);
#11117=ORIENTED_EDGE('',*,*,#8089,.T.);
#11118=ORIENTED_EDGE('',*,*,#8088,.F.);
#11119=ORIENTED_EDGE('',*,*,#8087,.T.);
#11120=ORIENTED_EDGE('',*,*,#8084,.T.);
#11121=ORIENTED_EDGE('',*,*,#8089,.F.);
#11122=ORIENTED_EDGE('',*,*,#8086,.F.);
#11123=ORIENTED_EDGE('',*,*,#8090,.F.);
#11124=ORIENTED_EDGE('',*,*,#8091,.F.);
#11125=ORIENTED_EDGE('',*,*,#8092,.F.);
#11126=ORIENTED_EDGE('',*,*,#8093,.F.);
#11127=ORIENTED_EDGE('',*,*,#8094,.F.);
#11128=ORIENTED_EDGE('',*,*,#8095,.T.);
#11129=ORIENTED_EDGE('',*,*,#8096,.F.);
#11130=ORIENTED_EDGE('',*,*,#8091,.T.);
#11131=ORIENTED_EDGE('',*,*,#8097,.F.);
#11132=ORIENTED_EDGE('',*,*,#8098,.F.);
#11133=ORIENTED_EDGE('',*,*,#8099,.F.);
#11134=ORIENTED_EDGE('',*,*,#8095,.F.);
#11135=ORIENTED_EDGE('',*,*,#8100,.T.);
#11136=ORIENTED_EDGE('',*,*,#8101,.T.);
#11137=ORIENTED_EDGE('',*,*,#8102,.T.);
#11138=ORIENTED_EDGE('',*,*,#8103,.T.);
#11139=ORIENTED_EDGE('',*,*,#8104,.T.);
#11140=ORIENTED_EDGE('',*,*,#8105,.T.);
#11141=ORIENTED_EDGE('',*,*,#8106,.T.);
#11142=ORIENTED_EDGE('',*,*,#8107,.T.);
#11143=ORIENTED_EDGE('',*,*,#8108,.T.);
#11144=ORIENTED_EDGE('',*,*,#8109,.T.);
#11145=ORIENTED_EDGE('',*,*,#8110,.T.);
#11146=ORIENTED_EDGE('',*,*,#8111,.T.);
#11147=ORIENTED_EDGE('',*,*,#8112,.T.);
#11148=ORIENTED_EDGE('',*,*,#8113,.T.);
#11149=ORIENTED_EDGE('',*,*,#8114,.T.);
#11150=ORIENTED_EDGE('',*,*,#8115,.T.);
#11151=ORIENTED_EDGE('',*,*,#8116,.T.);
#11152=ORIENTED_EDGE('',*,*,#8117,.T.);
#11153=ORIENTED_EDGE('',*,*,#8118,.T.);
#11154=ORIENTED_EDGE('',*,*,#8119,.T.);
#11155=ORIENTED_EDGE('',*,*,#8120,.T.);
#11156=ORIENTED_EDGE('',*,*,#8121,.T.);
#11157=ORIENTED_EDGE('',*,*,#8122,.T.);
#11158=ORIENTED_EDGE('',*,*,#8123,.T.);
#11159=ORIENTED_EDGE('',*,*,#8124,.T.);
#11160=ORIENTED_EDGE('',*,*,#8125,.T.);
#11161=ORIENTED_EDGE('',*,*,#8126,.T.);
#11162=ORIENTED_EDGE('',*,*,#8127,.T.);
#11163=ORIENTED_EDGE('',*,*,#8128,.T.);
#11164=ORIENTED_EDGE('',*,*,#8129,.T.);
#11165=ORIENTED_EDGE('',*,*,#8130,.T.);
#11166=ORIENTED_EDGE('',*,*,#8131,.T.);
#11167=ORIENTED_EDGE('',*,*,#8132,.T.);
#11168=ORIENTED_EDGE('',*,*,#8133,.T.);
#11169=ORIENTED_EDGE('',*,*,#8134,.T.);
#11170=ORIENTED_EDGE('',*,*,#8135,.T.);
#11171=ORIENTED_EDGE('',*,*,#8136,.T.);
#11172=ORIENTED_EDGE('',*,*,#8137,.T.);
#11173=ORIENTED_EDGE('',*,*,#8138,.T.);
#11174=ORIENTED_EDGE('',*,*,#8139,.T.);
#11175=ORIENTED_EDGE('',*,*,#8140,.T.);
#11176=ORIENTED_EDGE('',*,*,#8141,.T.);
#11177=ORIENTED_EDGE('',*,*,#8142,.T.);
#11178=ORIENTED_EDGE('',*,*,#8143,.T.);
#11179=ORIENTED_EDGE('',*,*,#8144,.T.);
#11180=ORIENTED_EDGE('',*,*,#8145,.T.);
#11181=ORIENTED_EDGE('',*,*,#8146,.T.);
#11182=ORIENTED_EDGE('',*,*,#8147,.T.);
#11183=ORIENTED_EDGE('',*,*,#8148,.T.);
#11184=ORIENTED_EDGE('',*,*,#8149,.T.);
#11185=ORIENTED_EDGE('',*,*,#8150,.T.);
#11186=ORIENTED_EDGE('',*,*,#8151,.T.);
#11187=ORIENTED_EDGE('',*,*,#8152,.T.);
#11188=ORIENTED_EDGE('',*,*,#8153,.T.);
#11189=ORIENTED_EDGE('',*,*,#8154,.T.);
#11190=ORIENTED_EDGE('',*,*,#8155,.T.);
#11191=ORIENTED_EDGE('',*,*,#8156,.T.);
#11192=ORIENTED_EDGE('',*,*,#8157,.T.);
#11193=ORIENTED_EDGE('',*,*,#8158,.T.);
#11194=ORIENTED_EDGE('',*,*,#8159,.T.);
#11195=ORIENTED_EDGE('',*,*,#8160,.T.);
#11196=ORIENTED_EDGE('',*,*,#8161,.T.);
#11197=ORIENTED_EDGE('',*,*,#8162,.T.);
#11198=ORIENTED_EDGE('',*,*,#8163,.T.);
#11199=ORIENTED_EDGE('',*,*,#8164,.T.);
#11200=ORIENTED_EDGE('',*,*,#8165,.T.);
#11201=ORIENTED_EDGE('',*,*,#8166,.T.);
#11202=ORIENTED_EDGE('',*,*,#8167,.T.);
#11203=ORIENTED_EDGE('',*,*,#8168,.T.);
#11204=ORIENTED_EDGE('',*,*,#8169,.T.);
#11205=ORIENTED_EDGE('',*,*,#8170,.T.);
#11206=ORIENTED_EDGE('',*,*,#8171,.T.);
#11207=ORIENTED_EDGE('',*,*,#8172,.T.);
#11208=ORIENTED_EDGE('',*,*,#8173,.T.);
#11209=ORIENTED_EDGE('',*,*,#8174,.T.);
#11210=ORIENTED_EDGE('',*,*,#8175,.T.);
#11211=ORIENTED_EDGE('',*,*,#8176,.T.);
#11212=ORIENTED_EDGE('',*,*,#8177,.T.);
#11213=ORIENTED_EDGE('',*,*,#8178,.T.);
#11214=ORIENTED_EDGE('',*,*,#8179,.T.);
#11215=ORIENTED_EDGE('',*,*,#8092,.T.);
#11216=ORIENTED_EDGE('',*,*,#8096,.T.);
#11217=ORIENTED_EDGE('',*,*,#8099,.T.);
#11218=ORIENTED_EDGE('',*,*,#8180,.T.);
#11219=ORIENTED_EDGE('',*,*,#8093,.T.);
#11220=ORIENTED_EDGE('',*,*,#8180,.F.);
#11221=ORIENTED_EDGE('',*,*,#8098,.T.);
#11222=ORIENTED_EDGE('',*,*,#8181,.F.);
#11223=ORIENTED_EDGE('',*,*,#8182,.F.);
#11224=ORIENTED_EDGE('',*,*,#8183,.T.);
#11225=ORIENTED_EDGE('',*,*,#8184,.F.);
#11226=ORIENTED_EDGE('',*,*,#8183,.F.);
#11227=ORIENTED_EDGE('',*,*,#8182,.T.);
#11228=ORIENTED_EDGE('',*,*,#8090,.T.);
#11229=ORIENTED_EDGE('',*,*,#8181,.T.);
#11230=ORIENTED_EDGE('',*,*,#8097,.T.);
#11231=ORIENTED_EDGE('',*,*,#8094,.T.);
#11232=ORIENTED_EDGE('',*,*,#8185,.F.);
#11233=ORIENTED_EDGE('',*,*,#8186,.F.);
#11234=ORIENTED_EDGE('',*,*,#8187,.F.);
#11235=ORIENTED_EDGE('',*,*,#8177,.F.);
#11236=ORIENTED_EDGE('',*,*,#8187,.T.);
#11237=ORIENTED_EDGE('',*,*,#8188,.F.);
#11238=ORIENTED_EDGE('',*,*,#8189,.F.);
#11239=ORIENTED_EDGE('',*,*,#8178,.F.);
#11240=ORIENTED_EDGE('',*,*,#8189,.T.);
#11241=ORIENTED_EDGE('',*,*,#8190,.F.);
#11242=ORIENTED_EDGE('',*,*,#8191,.F.);
#11243=ORIENTED_EDGE('',*,*,#8179,.F.);
#11244=ORIENTED_EDGE('',*,*,#8191,.T.);
#11245=ORIENTED_EDGE('',*,*,#8192,.F.);
#11246=ORIENTED_EDGE('',*,*,#8193,.T.);
#11247=ORIENTED_EDGE('',*,*,#8100,.F.);
#11248=ORIENTED_EDGE('',*,*,#8193,.F.);
#11249=ORIENTED_EDGE('',*,*,#8194,.F.);
#11250=ORIENTED_EDGE('',*,*,#8195,.F.);
#11251=ORIENTED_EDGE('',*,*,#8101,.F.);
#11252=ORIENTED_EDGE('',*,*,#8195,.T.);
#11253=ORIENTED_EDGE('',*,*,#8196,.F.);
#11254=ORIENTED_EDGE('',*,*,#8197,.F.);
#11255=ORIENTED_EDGE('',*,*,#8102,.F.);
#11256=ORIENTED_EDGE('',*,*,#8197,.T.);
#11257=ORIENTED_EDGE('',*,*,#8198,.F.);
#11258=ORIENTED_EDGE('',*,*,#8199,.F.);
#11259=ORIENTED_EDGE('',*,*,#8103,.F.);
#11260=ORIENTED_EDGE('',*,*,#8199,.T.);
#11261=ORIENTED_EDGE('',*,*,#8200,.F.);
#11262=ORIENTED_EDGE('',*,*,#8201,.T.);
#11263=ORIENTED_EDGE('',*,*,#8104,.F.);
#11264=ORIENTED_EDGE('',*,*,#8201,.F.);
#11265=ORIENTED_EDGE('',*,*,#8202,.F.);
#11266=ORIENTED_EDGE('',*,*,#8203,.F.);
#11267=ORIENTED_EDGE('',*,*,#8105,.F.);
#11268=ORIENTED_EDGE('',*,*,#8203,.T.);
#11269=ORIENTED_EDGE('',*,*,#8204,.F.);
#11270=ORIENTED_EDGE('',*,*,#8205,.F.);
#11271=ORIENTED_EDGE('',*,*,#8106,.F.);
#11272=ORIENTED_EDGE('',*,*,#8205,.T.);
#11273=ORIENTED_EDGE('',*,*,#8206,.F.);
#11274=ORIENTED_EDGE('',*,*,#8207,.F.);
#11275=ORIENTED_EDGE('',*,*,#8107,.F.);
#11276=ORIENTED_EDGE('',*,*,#8207,.T.);
#11277=ORIENTED_EDGE('',*,*,#8208,.F.);
#11278=ORIENTED_EDGE('',*,*,#8209,.T.);
#11279=ORIENTED_EDGE('',*,*,#8108,.F.);
#11280=ORIENTED_EDGE('',*,*,#8209,.F.);
#11281=ORIENTED_EDGE('',*,*,#8210,.F.);
#11282=ORIENTED_EDGE('',*,*,#8211,.F.);
#11283=ORIENTED_EDGE('',*,*,#8109,.F.);
#11284=ORIENTED_EDGE('',*,*,#8211,.T.);
#11285=ORIENTED_EDGE('',*,*,#8212,.F.);
#11286=ORIENTED_EDGE('',*,*,#8213,.F.);
#11287=ORIENTED_EDGE('',*,*,#8110,.F.);
#11288=ORIENTED_EDGE('',*,*,#8213,.T.);
#11289=ORIENTED_EDGE('',*,*,#8214,.F.);
#11290=ORIENTED_EDGE('',*,*,#8215,.F.);
#11291=ORIENTED_EDGE('',*,*,#8111,.F.);
#11292=ORIENTED_EDGE('',*,*,#8215,.T.);
#11293=ORIENTED_EDGE('',*,*,#8216,.F.);
#11294=ORIENTED_EDGE('',*,*,#8217,.T.);
#11295=ORIENTED_EDGE('',*,*,#8112,.F.);
#11296=ORIENTED_EDGE('',*,*,#8217,.F.);
#11297=ORIENTED_EDGE('',*,*,#8218,.F.);
#11298=ORIENTED_EDGE('',*,*,#8219,.F.);
#11299=ORIENTED_EDGE('',*,*,#8113,.F.);
#11300=ORIENTED_EDGE('',*,*,#8219,.T.);
#11301=ORIENTED_EDGE('',*,*,#8220,.F.);
#11302=ORIENTED_EDGE('',*,*,#8221,.F.);
#11303=ORIENTED_EDGE('',*,*,#8114,.F.);
#11304=ORIENTED_EDGE('',*,*,#8221,.T.);
#11305=ORIENTED_EDGE('',*,*,#8222,.F.);
#11306=ORIENTED_EDGE('',*,*,#8223,.F.);
#11307=ORIENTED_EDGE('',*,*,#8115,.F.);
#11308=ORIENTED_EDGE('',*,*,#8223,.T.);
#11309=ORIENTED_EDGE('',*,*,#8224,.F.);
#11310=ORIENTED_EDGE('',*,*,#8225,.T.);
#11311=ORIENTED_EDGE('',*,*,#8116,.F.);
#11312=ORIENTED_EDGE('',*,*,#8225,.F.);
#11313=ORIENTED_EDGE('',*,*,#8226,.F.);
#11314=ORIENTED_EDGE('',*,*,#8227,.F.);
#11315=ORIENTED_EDGE('',*,*,#8117,.F.);
#11316=ORIENTED_EDGE('',*,*,#8227,.T.);
#11317=ORIENTED_EDGE('',*,*,#8228,.F.);
#11318=ORIENTED_EDGE('',*,*,#8229,.F.);
#11319=ORIENTED_EDGE('',*,*,#8118,.F.);
#11320=ORIENTED_EDGE('',*,*,#8229,.T.);
#11321=ORIENTED_EDGE('',*,*,#8230,.F.);
#11322=ORIENTED_EDGE('',*,*,#8231,.F.);
#11323=ORIENTED_EDGE('',*,*,#8119,.F.);
#11324=ORIENTED_EDGE('',*,*,#8231,.T.);
#11325=ORIENTED_EDGE('',*,*,#8232,.F.);
#11326=ORIENTED_EDGE('',*,*,#8233,.T.);
#11327=ORIENTED_EDGE('',*,*,#8120,.F.);
#11328=ORIENTED_EDGE('',*,*,#8233,.F.);
#11329=ORIENTED_EDGE('',*,*,#8234,.F.);
#11330=ORIENTED_EDGE('',*,*,#8235,.F.);
#11331=ORIENTED_EDGE('',*,*,#8121,.F.);
#11332=ORIENTED_EDGE('',*,*,#8235,.T.);
#11333=ORIENTED_EDGE('',*,*,#8236,.F.);
#11334=ORIENTED_EDGE('',*,*,#8237,.F.);
#11335=ORIENTED_EDGE('',*,*,#8122,.F.);
#11336=ORIENTED_EDGE('',*,*,#8237,.T.);
#11337=ORIENTED_EDGE('',*,*,#8238,.F.);
#11338=ORIENTED_EDGE('',*,*,#8239,.F.);
#11339=ORIENTED_EDGE('',*,*,#8123,.F.);
#11340=ORIENTED_EDGE('',*,*,#8239,.T.);
#11341=ORIENTED_EDGE('',*,*,#8240,.F.);
#11342=ORIENTED_EDGE('',*,*,#8241,.T.);
#11343=ORIENTED_EDGE('',*,*,#8124,.F.);
#11344=ORIENTED_EDGE('',*,*,#8241,.F.);
#11345=ORIENTED_EDGE('',*,*,#8242,.F.);
#11346=ORIENTED_EDGE('',*,*,#8243,.F.);
#11347=ORIENTED_EDGE('',*,*,#8125,.F.);
#11348=ORIENTED_EDGE('',*,*,#8243,.T.);
#11349=ORIENTED_EDGE('',*,*,#8244,.F.);
#11350=ORIENTED_EDGE('',*,*,#8245,.F.);
#11351=ORIENTED_EDGE('',*,*,#8126,.F.);
#11352=ORIENTED_EDGE('',*,*,#8245,.T.);
#11353=ORIENTED_EDGE('',*,*,#8246,.F.);
#11354=ORIENTED_EDGE('',*,*,#8247,.F.);
#11355=ORIENTED_EDGE('',*,*,#8127,.F.);
#11356=ORIENTED_EDGE('',*,*,#8247,.T.);
#11357=ORIENTED_EDGE('',*,*,#8248,.F.);
#11358=ORIENTED_EDGE('',*,*,#8249,.T.);
#11359=ORIENTED_EDGE('',*,*,#8128,.F.);
#11360=ORIENTED_EDGE('',*,*,#8249,.F.);
#11361=ORIENTED_EDGE('',*,*,#8250,.F.);
#11362=ORIENTED_EDGE('',*,*,#8251,.F.);
#11363=ORIENTED_EDGE('',*,*,#8129,.F.);
#11364=ORIENTED_EDGE('',*,*,#8251,.T.);
#11365=ORIENTED_EDGE('',*,*,#8252,.F.);
#11366=ORIENTED_EDGE('',*,*,#8253,.F.);
#11367=ORIENTED_EDGE('',*,*,#8130,.F.);
#11368=ORIENTED_EDGE('',*,*,#8253,.T.);
#11369=ORIENTED_EDGE('',*,*,#8254,.F.);
#11370=ORIENTED_EDGE('',*,*,#8255,.F.);
#11371=ORIENTED_EDGE('',*,*,#8131,.F.);
#11372=ORIENTED_EDGE('',*,*,#8255,.T.);
#11373=ORIENTED_EDGE('',*,*,#8256,.F.);
#11374=ORIENTED_EDGE('',*,*,#8257,.T.);
#11375=ORIENTED_EDGE('',*,*,#8132,.F.);
#11376=ORIENTED_EDGE('',*,*,#8257,.F.);
#11377=ORIENTED_EDGE('',*,*,#8258,.F.);
#11378=ORIENTED_EDGE('',*,*,#8259,.F.);
#11379=ORIENTED_EDGE('',*,*,#8133,.F.);
#11380=ORIENTED_EDGE('',*,*,#8259,.T.);
#11381=ORIENTED_EDGE('',*,*,#8260,.F.);
#11382=ORIENTED_EDGE('',*,*,#8261,.F.);
#11383=ORIENTED_EDGE('',*,*,#8134,.F.);
#11384=ORIENTED_EDGE('',*,*,#8261,.T.);
#11385=ORIENTED_EDGE('',*,*,#8262,.F.);
#11386=ORIENTED_EDGE('',*,*,#8263,.F.);
#11387=ORIENTED_EDGE('',*,*,#8135,.F.);
#11388=ORIENTED_EDGE('',*,*,#8263,.T.);
#11389=ORIENTED_EDGE('',*,*,#8264,.F.);
#11390=ORIENTED_EDGE('',*,*,#8265,.T.);
#11391=ORIENTED_EDGE('',*,*,#8136,.F.);
#11392=ORIENTED_EDGE('',*,*,#8265,.F.);
#11393=ORIENTED_EDGE('',*,*,#8266,.F.);
#11394=ORIENTED_EDGE('',*,*,#8267,.F.);
#11395=ORIENTED_EDGE('',*,*,#8137,.F.);
#11396=ORIENTED_EDGE('',*,*,#8267,.T.);
#11397=ORIENTED_EDGE('',*,*,#8268,.F.);
#11398=ORIENTED_EDGE('',*,*,#8269,.F.);
#11399=ORIENTED_EDGE('',*,*,#8138,.F.);
#11400=ORIENTED_EDGE('',*,*,#8269,.T.);
#11401=ORIENTED_EDGE('',*,*,#8270,.F.);
#11402=ORIENTED_EDGE('',*,*,#8271,.F.);
#11403=ORIENTED_EDGE('',*,*,#8139,.F.);
#11404=ORIENTED_EDGE('',*,*,#8271,.T.);
#11405=ORIENTED_EDGE('',*,*,#8272,.F.);
#11406=ORIENTED_EDGE('',*,*,#8273,.T.);
#11407=ORIENTED_EDGE('',*,*,#8140,.F.);
#11408=ORIENTED_EDGE('',*,*,#8273,.F.);
#11409=ORIENTED_EDGE('',*,*,#8274,.F.);
#11410=ORIENTED_EDGE('',*,*,#8275,.F.);
#11411=ORIENTED_EDGE('',*,*,#8141,.F.);
#11412=ORIENTED_EDGE('',*,*,#8275,.T.);
#11413=ORIENTED_EDGE('',*,*,#8276,.F.);
#11414=ORIENTED_EDGE('',*,*,#8277,.F.);
#11415=ORIENTED_EDGE('',*,*,#8142,.F.);
#11416=ORIENTED_EDGE('',*,*,#8277,.T.);
#11417=ORIENTED_EDGE('',*,*,#8278,.F.);
#11418=ORIENTED_EDGE('',*,*,#8279,.F.);
#11419=ORIENTED_EDGE('',*,*,#8143,.F.);
#11420=ORIENTED_EDGE('',*,*,#8279,.T.);
#11421=ORIENTED_EDGE('',*,*,#8280,.F.);
#11422=ORIENTED_EDGE('',*,*,#8281,.T.);
#11423=ORIENTED_EDGE('',*,*,#8144,.F.);
#11424=ORIENTED_EDGE('',*,*,#8281,.F.);
#11425=ORIENTED_EDGE('',*,*,#8282,.F.);
#11426=ORIENTED_EDGE('',*,*,#8283,.F.);
#11427=ORIENTED_EDGE('',*,*,#8145,.F.);
#11428=ORIENTED_EDGE('',*,*,#8283,.T.);
#11429=ORIENTED_EDGE('',*,*,#8284,.F.);
#11430=ORIENTED_EDGE('',*,*,#8285,.F.);
#11431=ORIENTED_EDGE('',*,*,#8146,.F.);
#11432=ORIENTED_EDGE('',*,*,#8285,.T.);
#11433=ORIENTED_EDGE('',*,*,#8286,.F.);
#11434=ORIENTED_EDGE('',*,*,#8287,.F.);
#11435=ORIENTED_EDGE('',*,*,#8147,.F.);
#11436=ORIENTED_EDGE('',*,*,#8287,.T.);
#11437=ORIENTED_EDGE('',*,*,#8288,.F.);
#11438=ORIENTED_EDGE('',*,*,#8289,.T.);
#11439=ORIENTED_EDGE('',*,*,#8148,.F.);
#11440=ORIENTED_EDGE('',*,*,#8289,.F.);
#11441=ORIENTED_EDGE('',*,*,#8290,.F.);
#11442=ORIENTED_EDGE('',*,*,#8291,.F.);
#11443=ORIENTED_EDGE('',*,*,#8149,.F.);
#11444=ORIENTED_EDGE('',*,*,#8291,.T.);
#11445=ORIENTED_EDGE('',*,*,#8292,.F.);
#11446=ORIENTED_EDGE('',*,*,#8293,.F.);
#11447=ORIENTED_EDGE('',*,*,#8150,.F.);
#11448=ORIENTED_EDGE('',*,*,#8293,.T.);
#11449=ORIENTED_EDGE('',*,*,#8294,.F.);
#11450=ORIENTED_EDGE('',*,*,#8295,.F.);
#11451=ORIENTED_EDGE('',*,*,#8151,.F.);
#11452=ORIENTED_EDGE('',*,*,#8295,.T.);
#11453=ORIENTED_EDGE('',*,*,#8296,.F.);
#11454=ORIENTED_EDGE('',*,*,#8297,.T.);
#11455=ORIENTED_EDGE('',*,*,#8152,.F.);
#11456=ORIENTED_EDGE('',*,*,#8297,.F.);
#11457=ORIENTED_EDGE('',*,*,#8298,.F.);
#11458=ORIENTED_EDGE('',*,*,#8299,.F.);
#11459=ORIENTED_EDGE('',*,*,#8153,.F.);
#11460=ORIENTED_EDGE('',*,*,#8299,.T.);
#11461=ORIENTED_EDGE('',*,*,#8300,.F.);
#11462=ORIENTED_EDGE('',*,*,#8301,.F.);
#11463=ORIENTED_EDGE('',*,*,#8154,.F.);
#11464=ORIENTED_EDGE('',*,*,#8301,.T.);
#11465=ORIENTED_EDGE('',*,*,#8302,.F.);
#11466=ORIENTED_EDGE('',*,*,#8303,.F.);
#11467=ORIENTED_EDGE('',*,*,#8155,.F.);
#11468=ORIENTED_EDGE('',*,*,#8303,.T.);
#11469=ORIENTED_EDGE('',*,*,#8304,.F.);
#11470=ORIENTED_EDGE('',*,*,#8305,.T.);
#11471=ORIENTED_EDGE('',*,*,#8156,.F.);
#11472=ORIENTED_EDGE('',*,*,#8305,.F.);
#11473=ORIENTED_EDGE('',*,*,#8306,.F.);
#11474=ORIENTED_EDGE('',*,*,#8307,.F.);
#11475=ORIENTED_EDGE('',*,*,#8157,.F.);
#11476=ORIENTED_EDGE('',*,*,#8307,.T.);
#11477=ORIENTED_EDGE('',*,*,#8308,.F.);
#11478=ORIENTED_EDGE('',*,*,#8309,.F.);
#11479=ORIENTED_EDGE('',*,*,#8158,.F.);
#11480=ORIENTED_EDGE('',*,*,#8309,.T.);
#11481=ORIENTED_EDGE('',*,*,#8310,.F.);
#11482=ORIENTED_EDGE('',*,*,#8311,.F.);
#11483=ORIENTED_EDGE('',*,*,#8159,.F.);
#11484=ORIENTED_EDGE('',*,*,#8311,.T.);
#11485=ORIENTED_EDGE('',*,*,#8312,.F.);
#11486=ORIENTED_EDGE('',*,*,#8313,.T.);
#11487=ORIENTED_EDGE('',*,*,#8160,.F.);
#11488=ORIENTED_EDGE('',*,*,#8313,.F.);
#11489=ORIENTED_EDGE('',*,*,#8314,.F.);
#11490=ORIENTED_EDGE('',*,*,#8315,.F.);
#11491=ORIENTED_EDGE('',*,*,#8161,.F.);
#11492=ORIENTED_EDGE('',*,*,#8315,.T.);
#11493=ORIENTED_EDGE('',*,*,#8316,.F.);
#11494=ORIENTED_EDGE('',*,*,#8317,.F.);
#11495=ORIENTED_EDGE('',*,*,#8162,.F.);
#11496=ORIENTED_EDGE('',*,*,#8317,.T.);
#11497=ORIENTED_EDGE('',*,*,#8318,.F.);
#11498=ORIENTED_EDGE('',*,*,#8319,.F.);
#11499=ORIENTED_EDGE('',*,*,#8163,.F.);
#11500=ORIENTED_EDGE('',*,*,#8319,.T.);
#11501=ORIENTED_EDGE('',*,*,#8320,.F.);
#11502=ORIENTED_EDGE('',*,*,#8321,.T.);
#11503=ORIENTED_EDGE('',*,*,#8164,.F.);
#11504=ORIENTED_EDGE('',*,*,#8321,.F.);
#11505=ORIENTED_EDGE('',*,*,#8322,.F.);
#11506=ORIENTED_EDGE('',*,*,#8323,.F.);
#11507=ORIENTED_EDGE('',*,*,#8165,.F.);
#11508=ORIENTED_EDGE('',*,*,#8323,.T.);
#11509=ORIENTED_EDGE('',*,*,#8324,.F.);
#11510=ORIENTED_EDGE('',*,*,#8325,.F.);
#11511=ORIENTED_EDGE('',*,*,#8166,.F.);
#11512=ORIENTED_EDGE('',*,*,#8325,.T.);
#11513=ORIENTED_EDGE('',*,*,#8326,.F.);
#11514=ORIENTED_EDGE('',*,*,#8327,.F.);
#11515=ORIENTED_EDGE('',*,*,#8167,.F.);
#11516=ORIENTED_EDGE('',*,*,#8327,.T.);
#11517=ORIENTED_EDGE('',*,*,#8328,.F.);
#11518=ORIENTED_EDGE('',*,*,#8329,.T.);
#11519=ORIENTED_EDGE('',*,*,#8168,.F.);
#11520=ORIENTED_EDGE('',*,*,#8329,.F.);
#11521=ORIENTED_EDGE('',*,*,#8330,.F.);
#11522=ORIENTED_EDGE('',*,*,#8331,.F.);
#11523=ORIENTED_EDGE('',*,*,#8169,.F.);
#11524=ORIENTED_EDGE('',*,*,#8331,.T.);
#11525=ORIENTED_EDGE('',*,*,#8332,.F.);
#11526=ORIENTED_EDGE('',*,*,#8333,.F.);
#11527=ORIENTED_EDGE('',*,*,#8170,.F.);
#11528=ORIENTED_EDGE('',*,*,#8333,.T.);
#11529=ORIENTED_EDGE('',*,*,#8334,.F.);
#11530=ORIENTED_EDGE('',*,*,#8335,.F.);
#11531=ORIENTED_EDGE('',*,*,#8171,.F.);
#11532=ORIENTED_EDGE('',*,*,#8335,.T.);
#11533=ORIENTED_EDGE('',*,*,#8336,.F.);
#11534=ORIENTED_EDGE('',*,*,#8337,.T.);
#11535=ORIENTED_EDGE('',*,*,#8172,.F.);
#11536=ORIENTED_EDGE('',*,*,#8337,.F.);
#11537=ORIENTED_EDGE('',*,*,#8338,.F.);
#11538=ORIENTED_EDGE('',*,*,#8339,.F.);
#11539=ORIENTED_EDGE('',*,*,#8173,.F.);
#11540=ORIENTED_EDGE('',*,*,#8339,.T.);
#11541=ORIENTED_EDGE('',*,*,#8340,.F.);
#11542=ORIENTED_EDGE('',*,*,#8341,.F.);
#11543=ORIENTED_EDGE('',*,*,#8174,.F.);
#11544=ORIENTED_EDGE('',*,*,#8341,.T.);
#11545=ORIENTED_EDGE('',*,*,#8342,.F.);
#11546=ORIENTED_EDGE('',*,*,#8343,.F.);
#11547=ORIENTED_EDGE('',*,*,#8175,.F.);
#11548=ORIENTED_EDGE('',*,*,#8344,.T.);
#11549=ORIENTED_EDGE('',*,*,#8342,.T.);
#11550=ORIENTED_EDGE('',*,*,#8340,.T.);
#11551=ORIENTED_EDGE('',*,*,#8338,.T.);
#11552=ORIENTED_EDGE('',*,*,#8336,.T.);
#11553=ORIENTED_EDGE('',*,*,#8334,.T.);
#11554=ORIENTED_EDGE('',*,*,#8332,.T.);
#11555=ORIENTED_EDGE('',*,*,#8330,.T.);
#11556=ORIENTED_EDGE('',*,*,#8328,.T.);
#11557=ORIENTED_EDGE('',*,*,#8326,.T.);
#11558=ORIENTED_EDGE('',*,*,#8324,.T.);
#11559=ORIENTED_EDGE('',*,*,#8322,.T.);
#11560=ORIENTED_EDGE('',*,*,#8320,.T.);
#11561=ORIENTED_EDGE('',*,*,#8318,.T.);
#11562=ORIENTED_EDGE('',*,*,#8316,.T.);
#11563=ORIENTED_EDGE('',*,*,#8314,.T.);
#11564=ORIENTED_EDGE('',*,*,#8312,.T.);
#11565=ORIENTED_EDGE('',*,*,#8310,.T.);
#11566=ORIENTED_EDGE('',*,*,#8308,.T.);
#11567=ORIENTED_EDGE('',*,*,#8306,.T.);
#11568=ORIENTED_EDGE('',*,*,#8304,.T.);
#11569=ORIENTED_EDGE('',*,*,#8302,.T.);
#11570=ORIENTED_EDGE('',*,*,#8300,.T.);
#11571=ORIENTED_EDGE('',*,*,#8298,.T.);
#11572=ORIENTED_EDGE('',*,*,#8296,.T.);
#11573=ORIENTED_EDGE('',*,*,#8294,.T.);
#11574=ORIENTED_EDGE('',*,*,#8292,.T.);
#11575=ORIENTED_EDGE('',*,*,#8290,.T.);
#11576=ORIENTED_EDGE('',*,*,#8288,.T.);
#11577=ORIENTED_EDGE('',*,*,#8286,.T.);
#11578=ORIENTED_EDGE('',*,*,#8284,.T.);
#11579=ORIENTED_EDGE('',*,*,#8282,.T.);
#11580=ORIENTED_EDGE('',*,*,#8280,.T.);
#11581=ORIENTED_EDGE('',*,*,#8278,.T.);
#11582=ORIENTED_EDGE('',*,*,#8276,.T.);
#11583=ORIENTED_EDGE('',*,*,#8274,.T.);
#11584=ORIENTED_EDGE('',*,*,#8272,.T.);
#11585=ORIENTED_EDGE('',*,*,#8270,.T.);
#11586=ORIENTED_EDGE('',*,*,#8268,.T.);
#11587=ORIENTED_EDGE('',*,*,#8266,.T.);
#11588=ORIENTED_EDGE('',*,*,#8264,.T.);
#11589=ORIENTED_EDGE('',*,*,#8262,.T.);
#11590=ORIENTED_EDGE('',*,*,#8260,.T.);
#11591=ORIENTED_EDGE('',*,*,#8258,.T.);
#11592=ORIENTED_EDGE('',*,*,#8256,.T.);
#11593=ORIENTED_EDGE('',*,*,#8254,.T.);
#11594=ORIENTED_EDGE('',*,*,#8252,.T.);
#11595=ORIENTED_EDGE('',*,*,#8250,.T.);
#11596=ORIENTED_EDGE('',*,*,#8248,.T.);
#11597=ORIENTED_EDGE('',*,*,#8246,.T.);
#11598=ORIENTED_EDGE('',*,*,#8244,.T.);
#11599=ORIENTED_EDGE('',*,*,#8242,.T.);
#11600=ORIENTED_EDGE('',*,*,#8240,.T.);
#11601=ORIENTED_EDGE('',*,*,#8238,.T.);
#11602=ORIENTED_EDGE('',*,*,#8236,.T.);
#11603=ORIENTED_EDGE('',*,*,#8234,.T.);
#11604=ORIENTED_EDGE('',*,*,#8232,.T.);
#11605=ORIENTED_EDGE('',*,*,#8230,.T.);
#11606=ORIENTED_EDGE('',*,*,#8228,.T.);
#11607=ORIENTED_EDGE('',*,*,#8226,.T.);
#11608=ORIENTED_EDGE('',*,*,#8224,.T.);
#11609=ORIENTED_EDGE('',*,*,#8222,.T.);
#11610=ORIENTED_EDGE('',*,*,#8220,.T.);
#11611=ORIENTED_EDGE('',*,*,#8218,.T.);
#11612=ORIENTED_EDGE('',*,*,#8216,.T.);
#11613=ORIENTED_EDGE('',*,*,#8214,.T.);
#11614=ORIENTED_EDGE('',*,*,#8212,.T.);
#11615=ORIENTED_EDGE('',*,*,#8210,.T.);
#11616=ORIENTED_EDGE('',*,*,#8208,.T.);
#11617=ORIENTED_EDGE('',*,*,#8206,.T.);
#11618=ORIENTED_EDGE('',*,*,#8204,.T.);
#11619=ORIENTED_EDGE('',*,*,#8202,.T.);
#11620=ORIENTED_EDGE('',*,*,#8200,.T.);
#11621=ORIENTED_EDGE('',*,*,#8198,.T.);
#11622=ORIENTED_EDGE('',*,*,#8196,.T.);
#11623=ORIENTED_EDGE('',*,*,#8194,.T.);
#11624=ORIENTED_EDGE('',*,*,#8192,.T.);
#11625=ORIENTED_EDGE('',*,*,#8190,.T.);
#11626=ORIENTED_EDGE('',*,*,#8188,.T.);
#11627=ORIENTED_EDGE('',*,*,#8186,.T.);
#11628=ORIENTED_EDGE('',*,*,#8184,.T.);
#11629=ORIENTED_EDGE('',*,*,#8185,.T.);
#11630=ORIENTED_EDGE('',*,*,#8176,.F.);
#11631=ORIENTED_EDGE('',*,*,#8343,.T.);
#11632=ORIENTED_EDGE('',*,*,#8344,.F.);
#11633=ORIENTED_EDGE('',*,*,#8345,.F.);
#11634=ORIENTED_EDGE('',*,*,#8346,.T.);
#11635=ORIENTED_EDGE('',*,*,#8347,.T.);
#11636=ORIENTED_EDGE('',*,*,#8346,.F.);
#11637=ORIENTED_EDGE('',*,*,#8348,.F.);
#11638=ORIENTED_EDGE('',*,*,#8349,.T.);
#11639=ORIENTED_EDGE('',*,*,#8350,.T.);
#11640=ORIENTED_EDGE('',*,*,#8349,.F.);
#11641=ORIENTED_EDGE('',*,*,#8348,.T.);
#11642=ORIENTED_EDGE('',*,*,#8345,.T.);
#11643=ORIENTED_EDGE('',*,*,#8350,.F.);
#11644=ORIENTED_EDGE('',*,*,#8347,.F.);
#11645=ORIENTED_EDGE('',*,*,#8351,.F.);
#11646=ORIENTED_EDGE('',*,*,#8352,.F.);
#11647=ORIENTED_EDGE('',*,*,#8353,.T.);
#11648=ORIENTED_EDGE('',*,*,#8351,.T.);
#11649=ORIENTED_EDGE('',*,*,#8353,.F.);
#11650=ORIENTED_EDGE('',*,*,#8354,.F.);
#11651=ORIENTED_EDGE('',*,*,#8355,.T.);
#11652=ORIENTED_EDGE('',*,*,#8352,.T.);
#11653=ORIENTED_EDGE('',*,*,#8355,.F.);
#11654=ORIENTED_EDGE('',*,*,#8356,.F.);
#11655=ORIENTED_EDGE('',*,*,#8357,.T.);
#11656=ORIENTED_EDGE('',*,*,#8354,.T.);
#11657=ORIENTED_EDGE('',*,*,#8357,.F.);
#11658=ORIENTED_EDGE('',*,*,#8356,.T.);
#11659=ORIENTED_EDGE('',*,*,#8358,.F.);
#11660=ORIENTED_EDGE('',*,*,#8359,.F.);
#11661=ORIENTED_EDGE('',*,*,#8360,.T.);
#11662=ORIENTED_EDGE('',*,*,#8358,.T.);
#11663=ORIENTED_EDGE('',*,*,#8360,.F.);
#11664=ORIENTED_EDGE('',*,*,#8361,.F.);
#11665=ORIENTED_EDGE('',*,*,#8362,.T.);
#11666=ORIENTED_EDGE('',*,*,#8359,.T.);
#11667=ORIENTED_EDGE('',*,*,#8362,.F.);
#11668=ORIENTED_EDGE('',*,*,#8363,.F.);
#11669=ORIENTED_EDGE('',*,*,#8364,.T.);
#11670=ORIENTED_EDGE('',*,*,#8361,.T.);
#11671=ORIENTED_EDGE('',*,*,#8364,.F.);
#11672=ORIENTED_EDGE('',*,*,#8363,.T.);
#11673=ORIENTED_EDGE('',*,*,#8365,.T.);
#11674=ORIENTED_EDGE('',*,*,#8366,.T.);
#11675=ORIENTED_EDGE('',*,*,#8367,.T.);
#11676=ORIENTED_EDGE('',*,*,#8368,.F.);
#11677=ORIENTED_EDGE('',*,*,#8369,.T.);
#11678=ORIENTED_EDGE('',*,*,#8370,.T.);
#11679=ORIENTED_EDGE('',*,*,#8371,.T.);
#11680=ORIENTED_EDGE('',*,*,#8366,.F.);
#11681=ORIENTED_EDGE('',*,*,#8372,.T.);
#11682=ORIENTED_EDGE('',*,*,#8373,.T.);
#11683=ORIENTED_EDGE('',*,*,#8374,.T.);
#11684=ORIENTED_EDGE('',*,*,#8370,.F.);
#11685=ORIENTED_EDGE('',*,*,#8375,.T.);
#11686=ORIENTED_EDGE('',*,*,#8376,.T.);
#11687=ORIENTED_EDGE('',*,*,#8377,.T.);
#11688=ORIENTED_EDGE('',*,*,#8373,.F.);
#11689=ORIENTED_EDGE('',*,*,#8378,.T.);
#11690=ORIENTED_EDGE('',*,*,#8379,.T.);
#11691=ORIENTED_EDGE('',*,*,#8380,.T.);
#11692=ORIENTED_EDGE('',*,*,#8376,.F.);
#11693=ORIENTED_EDGE('',*,*,#8381,.T.);
#11694=ORIENTED_EDGE('',*,*,#8368,.T.);
#11695=ORIENTED_EDGE('',*,*,#8382,.T.);
#11696=ORIENTED_EDGE('',*,*,#8379,.F.);
#11697=ORIENTED_EDGE('',*,*,#8381,.F.);
#11698=ORIENTED_EDGE('',*,*,#8378,.F.);
#11699=ORIENTED_EDGE('',*,*,#8375,.F.);
#11700=ORIENTED_EDGE('',*,*,#8372,.F.);
#11701=ORIENTED_EDGE('',*,*,#8369,.F.);
#11702=ORIENTED_EDGE('',*,*,#8365,.F.);
#11703=ORIENTED_EDGE('',*,*,#8382,.F.);
#11704=ORIENTED_EDGE('',*,*,#8367,.F.);
#11705=ORIENTED_EDGE('',*,*,#8371,.F.);
#11706=ORIENTED_EDGE('',*,*,#8374,.F.);
#11707=ORIENTED_EDGE('',*,*,#8377,.F.);
#11708=ORIENTED_EDGE('',*,*,#8380,.F.);
#11709=ORIENTED_EDGE('',*,*,#8383,.F.);
#11710=ORIENTED_EDGE('',*,*,#8384,.F.);
#11711=ORIENTED_EDGE('',*,*,#8385,.T.);
#11712=ORIENTED_EDGE('',*,*,#8383,.T.);
#11713=ORIENTED_EDGE('',*,*,#8385,.F.);
#11714=ORIENTED_EDGE('',*,*,#8386,.F.);
#11715=ORIENTED_EDGE('',*,*,#8387,.T.);
#11716=ORIENTED_EDGE('',*,*,#8384,.T.);
#11717=ORIENTED_EDGE('',*,*,#8387,.F.);
#11718=ORIENTED_EDGE('',*,*,#8388,.F.);
#11719=ORIENTED_EDGE('',*,*,#8389,.T.);
#11720=ORIENTED_EDGE('',*,*,#8386,.T.);
#11721=ORIENTED_EDGE('',*,*,#8389,.F.);
#11722=ORIENTED_EDGE('',*,*,#8388,.T.);
#11723=ORIENTED_EDGE('',*,*,#8390,.F.);
#11724=ORIENTED_EDGE('',*,*,#8391,.F.);
#11725=ORIENTED_EDGE('',*,*,#8392,.T.);
#11726=ORIENTED_EDGE('',*,*,#8390,.T.);
#11727=ORIENTED_EDGE('',*,*,#8392,.F.);
#11728=ORIENTED_EDGE('',*,*,#8393,.F.);
#11729=ORIENTED_EDGE('',*,*,#8394,.T.);
#11730=ORIENTED_EDGE('',*,*,#8391,.T.);
#11731=ORIENTED_EDGE('',*,*,#8394,.F.);
#11732=ORIENTED_EDGE('',*,*,#8395,.F.);
#11733=ORIENTED_EDGE('',*,*,#8396,.T.);
#11734=ORIENTED_EDGE('',*,*,#8393,.T.);
#11735=ORIENTED_EDGE('',*,*,#8396,.F.);
#11736=ORIENTED_EDGE('',*,*,#8395,.T.);
#11737=ORIENTED_EDGE('',*,*,#8397,.T.);
#11738=ORIENTED_EDGE('',*,*,#8398,.T.);
#11739=ORIENTED_EDGE('',*,*,#8399,.T.);
#11740=ORIENTED_EDGE('',*,*,#8400,.F.);
#11741=ORIENTED_EDGE('',*,*,#8401,.T.);
#11742=ORIENTED_EDGE('',*,*,#8402,.T.);
#11743=ORIENTED_EDGE('',*,*,#8403,.T.);
#11744=ORIENTED_EDGE('',*,*,#8398,.F.);
#11745=ORIENTED_EDGE('',*,*,#8404,.T.);
#11746=ORIENTED_EDGE('',*,*,#8405,.T.);
#11747=ORIENTED_EDGE('',*,*,#8406,.T.);
#11748=ORIENTED_EDGE('',*,*,#8402,.F.);
#11749=ORIENTED_EDGE('',*,*,#8407,.T.);
#11750=ORIENTED_EDGE('',*,*,#8408,.T.);
#11751=ORIENTED_EDGE('',*,*,#8409,.T.);
#11752=ORIENTED_EDGE('',*,*,#8405,.F.);
#11753=ORIENTED_EDGE('',*,*,#8410,.T.);
#11754=ORIENTED_EDGE('',*,*,#8411,.T.);
#11755=ORIENTED_EDGE('',*,*,#8412,.T.);
#11756=ORIENTED_EDGE('',*,*,#8408,.F.);
#11757=ORIENTED_EDGE('',*,*,#8413,.T.);
#11758=ORIENTED_EDGE('',*,*,#8400,.T.);
#11759=ORIENTED_EDGE('',*,*,#8414,.T.);
#11760=ORIENTED_EDGE('',*,*,#8411,.F.);
#11761=ORIENTED_EDGE('',*,*,#8413,.F.);
#11762=ORIENTED_EDGE('',*,*,#8410,.F.);
#11763=ORIENTED_EDGE('',*,*,#8407,.F.);
#11764=ORIENTED_EDGE('',*,*,#8404,.F.);
#11765=ORIENTED_EDGE('',*,*,#8401,.F.);
#11766=ORIENTED_EDGE('',*,*,#8397,.F.);
#11767=ORIENTED_EDGE('',*,*,#8414,.F.);
#11768=ORIENTED_EDGE('',*,*,#8399,.F.);
#11769=ORIENTED_EDGE('',*,*,#8403,.F.);
#11770=ORIENTED_EDGE('',*,*,#8406,.F.);
#11771=ORIENTED_EDGE('',*,*,#8409,.F.);
#11772=ORIENTED_EDGE('',*,*,#8412,.F.);
#11773=ORIENTED_EDGE('',*,*,#8415,.F.);
#11774=ORIENTED_EDGE('',*,*,#8416,.T.);
#11775=ORIENTED_EDGE('',*,*,#8417,.T.);
#11776=ORIENTED_EDGE('',*,*,#8416,.F.);
#11777=ORIENTED_EDGE('',*,*,#8418,.F.);
#11778=ORIENTED_EDGE('',*,*,#8419,.T.);
#11779=ORIENTED_EDGE('',*,*,#8420,.T.);
#11780=ORIENTED_EDGE('',*,*,#8419,.F.);
#11781=ORIENTED_EDGE('',*,*,#8418,.T.);
#11782=ORIENTED_EDGE('',*,*,#8415,.T.);
#11783=ORIENTED_EDGE('',*,*,#8420,.F.);
#11784=ORIENTED_EDGE('',*,*,#8417,.F.);
#11785=CYLINDRICAL_SURFACE('',#13191,0.165);
#11786=CYLINDRICAL_SURFACE('',#13194,0.165);
#11787=CYLINDRICAL_SURFACE('',#13197,0.165);
#11788=CYLINDRICAL_SURFACE('',#13200,0.165);
#11789=CYLINDRICAL_SURFACE('',#13203,0.165);
#11790=CYLINDRICAL_SURFACE('',#13206,0.165);
#11791=CYLINDRICAL_SURFACE('',#13230,0.165);
#11792=CYLINDRICAL_SURFACE('',#13234,0.165);
#11793=CYLINDRICAL_SURFACE('',#13244,1.4);
#11794=CYLINDRICAL_SURFACE('',#13246,2.);
#11795=CYLINDRICAL_SURFACE('',#13248,2.);
#11796=CYLINDRICAL_SURFACE('',#13253,0.165);
#11797=CYLINDRICAL_SURFACE('',#13257,0.165);
#11798=CYLINDRICAL_SURFACE('',#13269,1.4);
#11799=CYLINDRICAL_SURFACE('',#13271,2.);
#11800=CYLINDRICAL_SURFACE('',#13273,2.);
#11801=CYLINDRICAL_SURFACE('',#13281,0.164999999999999);
#11802=CYLINDRICAL_SURFACE('',#13286,0.605);
#11803=CYLINDRICAL_SURFACE('',#13289,1.4);
#11804=CYLINDRICAL_SURFACE('',#13298,0.375);
#11805=CYLINDRICAL_SURFACE('',#13303,0.375);
#11806=CYLINDRICAL_SURFACE('',#13317,0.165);
#11807=CYLINDRICAL_SURFACE('',#13320,0.225);
#11808=CYLINDRICAL_SURFACE('',#13322,0.225);
#11809=CYLINDRICAL_SURFACE('',#13324,1.4);
#11810=CYLINDRICAL_SURFACE('',#13328,0.605);
#11811=CYLINDRICAL_SURFACE('',#13330,2.);
#11812=CYLINDRICAL_SURFACE('',#13341,1.005);
#11813=CYLINDRICAL_SURFACE('',#13343,1.4);
#11814=CYLINDRICAL_SURFACE('',#13347,1.6);
#11815=CYLINDRICAL_SURFACE('',#13351,0.225);
#11816=CYLINDRICAL_SURFACE('',#13354,0.225);
#11817=CYLINDRICAL_SURFACE('',#13365,1.01);
#11818=CYLINDRICAL_SURFACE('',#13379,1.005);
#11819=CYLINDRICAL_SURFACE('',#13381,1.4);
#11820=CYLINDRICAL_SURFACE('',#13385,1.6);
#11821=CYLINDRICAL_SURFACE('',#13389,0.225);
#11822=CYLINDRICAL_SURFACE('',#13392,0.225);
#11823=CYLINDRICAL_SURFACE('',#13403,1.01);
#11824=CYLINDRICAL_SURFACE('',#13422,0.165);
#11825=CYLINDRICAL_SURFACE('',#13425,0.5);
#11826=CYLINDRICAL_SURFACE('',#13426,0.605);
#11827=CYLINDRICAL_SURFACE('',#13428,1.4);
#11828=CYLINDRICAL_SURFACE('',#13432,0.165);
#11829=CYLINDRICAL_SURFACE('',#13435,0.165);
#11830=CYLINDRICAL_SURFACE('',#13438,0.165);
#11831=CYLINDRICAL_SURFACE('',#13441,0.165);
#11832=CYLINDRICAL_SURFACE('',#13444,0.225);
#11833=CYLINDRICAL_SURFACE('',#13447,0.225);
#11834=CYLINDRICAL_SURFACE('',#13450,1.6);
#11835=CYLINDRICAL_SURFACE('',#13464,0.225);
#11836=CYLINDRICAL_SURFACE('',#13467,0.225);
#11837=CYLINDRICAL_SURFACE('',#13470,0.225);
#11838=CYLINDRICAL_SURFACE('',#13473,0.225);
#11839=CYLINDRICAL_SURFACE('',#13476,1.59);
#11840=CYLINDRICAL_SURFACE('',#13481,1.41);
#11841=CYLINDRICAL_SURFACE('',#13483,2.4);
#11842=CYLINDRICAL_SURFACE('',#13489,0.225);
#11843=CYLINDRICAL_SURFACE('',#13492,0.225);
#11844=CYLINDRICAL_SURFACE('',#13495,0.225);
#11845=CYLINDRICAL_SURFACE('',#13498,0.225);
#11846=CYLINDRICAL_SURFACE('',#13501,1.59);
#11847=CYLINDRICAL_SURFACE('',#13506,1.41);
#11848=CYLINDRICAL_SURFACE('',#13508,2.4);
#11849=CYLINDRICAL_SURFACE('',#13514,0.165);
#11850=CYLINDRICAL_SURFACE('',#13517,0.165);
#11851=CYLINDRICAL_SURFACE('',#13520,0.165);
#11852=CYLINDRICAL_SURFACE('',#13523,0.165);
#11853=CYLINDRICAL_SURFACE('',#13526,0.225);
#11854=CYLINDRICAL_SURFACE('',#13529,0.225);
#11855=CYLINDRICAL_SURFACE('',#13532,1.6);
#11856=CYLINDRICAL_SURFACE('',#13546,0.225);
#11857=CYLINDRICAL_SURFACE('',#13549,0.225);
#11858=CYLINDRICAL_SURFACE('',#13552,0.225);
#11859=CYLINDRICAL_SURFACE('',#13555,0.225);
#11860=CYLINDRICAL_SURFACE('',#13558,1.59);
#11861=CYLINDRICAL_SURFACE('',#13563,1.41);
#11862=CYLINDRICAL_SURFACE('',#13565,2.4);
#11863=CYLINDRICAL_SURFACE('',#13571,0.225);
#11864=CYLINDRICAL_SURFACE('',#13574,0.225);
#11865=CYLINDRICAL_SURFACE('',#13577,0.225);
#11866=CYLINDRICAL_SURFACE('',#13580,0.225);
#11867=CYLINDRICAL_SURFACE('',#13583,1.59);
#11868=CYLINDRICAL_SURFACE('',#13588,1.41);
#11869=CYLINDRICAL_SURFACE('',#13590,2.4);
#11870=CYLINDRICAL_SURFACE('',#13601,0.6);
#11871=CYLINDRICAL_SURFACE('',#13611,1.070235);
#11872=CYLINDRICAL_SURFACE('',#13613,0.6);
#11873=CYLINDRICAL_SURFACE('',#13619,1.070235);
#11874=CYLINDRICAL_SURFACE('',#13631,1.129765);
#11875=CYLINDRICAL_SURFACE('',#13638,1.6);
#11876=CYLINDRICAL_SURFACE('',#13643,1.129765);
#11877=CYLINDRICAL_SURFACE('',#13663,1.123812);
#11878=CYLINDRICAL_SURFACE('',#13699,1.076188);
#11879=CYLINDRICAL_SURFACE('',#13713,1.119765);
#11880=CYLINDRICAL_SURFACE('',#13717,1.085235);
#11881=CYLINDRICAL_SURFACE('',#13721,1.119765);
#11882=CYLINDRICAL_SURFACE('',#13725,1.085235);
#11883=CYLINDRICAL_SURFACE('',#13746,0.35);
#11884=CYLINDRICAL_SURFACE('',#13754,0.1954);
#11885=CYLINDRICAL_SURFACE('',#13757,0.425);
#11886=CYLINDRICAL_SURFACE('',#13932,1.);
#11887=CYLINDRICAL_SURFACE('',#13940,0.164999999999999);
#11888=CYLINDRICAL_SURFACE('',#13943,0.3);
#11889=CYLINDRICAL_SURFACE('',#13946,0.5);
#11890=CYLINDRICAL_SURFACE('',#13950,1.4);
#11891=CYLINDRICAL_SURFACE('',#13956,0.3);
#11892=CYLINDRICAL_SURFACE('',#13962,0.199999999999999);
#11893=CYLINDRICAL_SURFACE('',#13968,0.164999999999999);
#11894=CYLINDRICAL_SURFACE('',#13976,1.7);
#11895=CYLINDRICAL_SURFACE('',#13978,1.005);
#11896=CYLINDRICAL_SURFACE('',#13993,0.1954);
#11897=CYLINDRICAL_SURFACE('',#14006,0.165);
#11898=CYLINDRICAL_SURFACE('',#14010,0.165);
#11899=CYLINDRICAL_SURFACE('',#14028,0.6);
#11900=CYLINDRICAL_SURFACE('',#14034,0.605);
#11901=CYLINDRICAL_SURFACE('',#14037,0.8);
#11902=CYLINDRICAL_SURFACE('',#14043,0.605);
#11903=CYLINDRICAL_SURFACE('',#14046,0.8);
#11904=CYLINDRICAL_SURFACE('',#14052,0.605);
#11905=CYLINDRICAL_SURFACE('',#14055,0.8);
#11906=CYLINDRICAL_SURFACE('',#14061,0.605);
#11907=CYLINDRICAL_SURFACE('',#14064,0.8);
#11908=CYLINDRICAL_SURFACE('',#14084,0.25);
#11909=CYLINDRICAL_SURFACE('',#14093,0.6);
#11910=CYLINDRICAL_SURFACE('',#14095,0.9);
#11911=CYLINDRICAL_SURFACE('',#14104,1.3);
#11912=CYLINDRICAL_SURFACE('',#14108,0.33);
#11913=CYLINDRICAL_SURFACE('',#14111,0.4);
#11914=CYLINDRICAL_SURFACE('',#14117,0.225);
#11915=CYLINDRICAL_SURFACE('',#14120,1.);
#11916=CYLINDRICAL_SURFACE('',#14126,0.225);
#11917=CYLINDRICAL_SURFACE('',#14129,1.);
#11918=CYLINDRICAL_SURFACE('',#14160,0.6);
#11919=CYLINDRICAL_SURFACE('',#14162,1.4);
#11920=CYLINDRICAL_SURFACE('',#14167,1.75);
#11921=CYLINDRICAL_SURFACE('',#14170,1.75);
#11922=CYLINDRICAL_SURFACE('',#14173,1.75);
#11923=CYLINDRICAL_SURFACE('',#14176,1.75);
#11924=CYLINDRICAL_SURFACE('',#14179,1.75);
#11925=CYLINDRICAL_SURFACE('',#14182,1.75);
#11926=CYLINDRICAL_SURFACE('',#14185,1.75);
#11927=CYLINDRICAL_SURFACE('',#14188,1.75);
#11928=CYLINDRICAL_SURFACE('',#14191,1.75);
#11929=CYLINDRICAL_SURFACE('',#14194,1.75);
#11930=CYLINDRICAL_SURFACE('',#14197,1.75);
#11931=CYLINDRICAL_SURFACE('',#14200,1.75);
#11932=CYLINDRICAL_SURFACE('',#14203,1.75);
#11933=CYLINDRICAL_SURFACE('',#14206,1.75);
#11934=CYLINDRICAL_SURFACE('',#14209,1.75);
#11935=CYLINDRICAL_SURFACE('',#14212,1.75);
#11936=CYLINDRICAL_SURFACE('',#14215,1.75);
#11937=CYLINDRICAL_SURFACE('',#14218,1.75);
#11938=CYLINDRICAL_SURFACE('',#14221,1.75);
#11939=CYLINDRICAL_SURFACE('',#14226,1.75);
#11940=CYLINDRICAL_SURFACE('',#14228,0.32);
#11941=CYLINDRICAL_SURFACE('',#14231,0.6);
#11942=CYLINDRICAL_SURFACE('',#14241,0.5);
#11943=CYLINDRICAL_SURFACE('',#14249,0.2942);
#11944=CYLINDRICAL_SURFACE('',#14267,0.35);
#11945=CYLINDRICAL_SURFACE('',#14275,0.1954);
#11946=CYLINDRICAL_SURFACE('',#14354,0.405);
#11947=CYLINDRICAL_SURFACE('',#14357,0.9);
#11948=ADVANCED_FACE('',(#1339),#11785,.F.);
#11949=ADVANCED_FACE('',(#1340),#11786,.F.);
#11950=ADVANCED_FACE('',(#1341),#11787,.F.);
#11951=ADVANCED_FACE('',(#1342),#11788,.F.);
#11952=ADVANCED_FACE('',(#1343),#11789,.F.);
#11953=ADVANCED_FACE('',(#1344),#11790,.F.);
#11954=ADVANCED_FACE('',(#1345),#887,.T.);
#11955=ADVANCED_FACE('',(#1346),#888,.T.);
#11956=ADVANCED_FACE('',(#1347),#889,.T.);
#11957=ADVANCED_FACE('',(#1348),#890,.T.);
#11958=ADVANCED_FACE('',(#1349,#720,#721,#722,#723,#724,#725),#891,.T.);
#11959=ADVANCED_FACE('',(#1350,#726,#727,#728,#729,#730,#731),#892,.F.);
#11960=ADVANCED_FACE('',(#1351),#893,.T.);
#11961=ADVANCED_FACE('',(#1352),#894,.T.);
#11962=ADVANCED_FACE('',(#1353),#895,.T.);
#11963=ADVANCED_FACE('',(#1354),#896,.T.);
#11964=ADVANCED_FACE('',(#1355),#897,.T.);
#11965=ADVANCED_FACE('',(#1356),#898,.F.);
#11966=ADVANCED_FACE('',(#1357),#899,.T.);
#11967=ADVANCED_FACE('',(#1358),#900,.T.);
#11968=ADVANCED_FACE('',(#1359),#901,.T.);
#11969=ADVANCED_FACE('',(#1360),#902,.T.);
#11970=ADVANCED_FACE('',(#1361),#903,.T.);
#11971=ADVANCED_FACE('',(#1362),#904,.F.);
#11972=ADVANCED_FACE('',(#1363),#11791,.F.);
#11973=ADVANCED_FACE('',(#1364),#905,.T.);
#11974=ADVANCED_FACE('',(#1365),#11792,.F.);
#11975=ADVANCED_FACE('',(#1366),#906,.T.);
#11976=ADVANCED_FACE('',(#1367),#907,.F.);
#11977=ADVANCED_FACE('',(#1368),#908,.F.);
#11978=ADVANCED_FACE('',(#1369),#909,.F.);
#11979=ADVANCED_FACE('',(#1370),#11793,.F.);
#11980=ADVANCED_FACE('',(#1371),#11794,.T.);
#11981=ADVANCED_FACE('',(#1372),#11795,.T.);
#11982=ADVANCED_FACE('',(#1373,#732,#733),#910,.T.);
#11983=ADVANCED_FACE('',(#1374),#911,.T.);
#11984=ADVANCED_FACE('',(#1375),#912,.T.);
#11985=ADVANCED_FACE('',(#1376),#11796,.F.);
#11986=ADVANCED_FACE('',(#1377),#913,.T.);
#11987=ADVANCED_FACE('',(#1378),#11797,.F.);
#11988=ADVANCED_FACE('',(#1379),#914,.T.);
#11989=ADVANCED_FACE('',(#1380),#915,.F.);
#11990=ADVANCED_FACE('',(#1381),#916,.F.);
#11991=ADVANCED_FACE('',(#1382),#917,.F.);
#11992=ADVANCED_FACE('',(#1383),#11798,.F.);
#11993=ADVANCED_FACE('',(#1384),#11799,.T.);
#11994=ADVANCED_FACE('',(#1385),#11800,.T.);
#11995=ADVANCED_FACE('',(#1386,#734,#735),#918,.T.);
#11996=ADVANCED_FACE('',(#1387),#919,.T.);
#11997=ADVANCED_FACE('',(#1388),#920,.T.);
#11998=ADVANCED_FACE('',(#1389,#736),#921,.T.);
#11999=ADVANCED_FACE('',(#1390),#922,.T.);
#12000=ADVANCED_FACE('',(#1391),#11801,.F.);
#12001=ADVANCED_FACE('',(#1392),#923,.T.);
#12002=ADVANCED_FACE('',(#1393),#924,.T.);
#12003=ADVANCED_FACE('',(#1394,#737),#11802,.F.);
#12004=ADVANCED_FACE('',(#1395,#738),#11803,.T.);
#12005=ADVANCED_FACE('',(#1396,#739),#925,.F.);
#12006=ADVANCED_FACE('',(#1397),#926,.T.);
#12007=ADVANCED_FACE('',(#1398),#927,.T.);
#12008=ADVANCED_FACE('',(#1399),#928,.T.);
#12009=ADVANCED_FACE('',(#1400),#929,.T.);
#12010=ADVANCED_FACE('',(#1401),#930,.F.);
#12011=ADVANCED_FACE('',(#1402),#11804,.F.);
#12012=ADVANCED_FACE('',(#1403),#931,.F.);
#12013=ADVANCED_FACE('',(#1404),#11805,.F.);
#12014=ADVANCED_FACE('',(#1405),#932,.F.);
#12015=ADVANCED_FACE('',(#1406,#740,#741,#742),#933,.T.);
#12016=ADVANCED_FACE('',(#1407),#934,.T.);
#12017=ADVANCED_FACE('',(#1408),#11806,.F.);
#12018=ADVANCED_FACE('',(#1409),#935,.T.);
#12019=ADVANCED_FACE('',(#1410),#11807,.F.);
#12020=ADVANCED_FACE('',(#1411),#11808,.F.);
#12021=ADVANCED_FACE('',(#1412,#743),#11809,.T.);
#12022=ADVANCED_FACE('',(#1413,#744),#936,.T.);
#12023=ADVANCED_FACE('',(#1414,#745),#11810,.F.);
#12024=ADVANCED_FACE('',(#1415),#11811,.T.);
#12025=ADVANCED_FACE('',(#1416,#746,#747,#748),#937,.F.);
#12026=ADVANCED_FACE('',(#1417),#938,.F.);
#12027=ADVANCED_FACE('',(#1418),#939,.F.);
#12028=ADVANCED_FACE('',(#1419),#940,.F.);
#12029=ADVANCED_FACE('',(#1420),#941,.F.);
#12030=ADVANCED_FACE('',(#1421),#942,.F.);
#12031=ADVANCED_FACE('',(#1422),#11812,.F.);
#12032=ADVANCED_FACE('',(#1423),#11813,.T.);
#12033=ADVANCED_FACE('',(#1424),#943,.F.);
#12034=ADVANCED_FACE('',(#1425),#11814,.T.);
#12035=ADVANCED_FACE('',(#1426),#944,.T.);
#12036=ADVANCED_FACE('',(#1427),#11815,.F.);
#12037=ADVANCED_FACE('',(#1428),#11816,.F.);
#12038=ADVANCED_FACE('',(#1429),#945,.F.);
#12039=ADVANCED_FACE('',(#1430),#946,.F.);
#12040=ADVANCED_FACE('',(#1431),#947,.F.);
#12041=ADVANCED_FACE('',(#1432),#948,.F.);
#12042=ADVANCED_FACE('',(#1433),#949,.T.);
#12043=ADVANCED_FACE('',(#1434),#950,.T.);
#12044=ADVANCED_FACE('',(#1435,#749,#750),#951,.T.);
#12045=ADVANCED_FACE('',(#1436),#11817,.F.);
#12046=ADVANCED_FACE('',(#1437),#952,.T.);
#12047=ADVANCED_FACE('',(#1438),#953,.T.);
#12048=ADVANCED_FACE('',(#1439),#954,.T.);
#12049=ADVANCED_FACE('',(#1440,#751,#752),#955,.F.);
#12050=ADVANCED_FACE('',(#1441),#956,.F.);
#12051=ADVANCED_FACE('',(#1442),#957,.F.);
#12052=ADVANCED_FACE('',(#1443),#958,.F.);
#12053=ADVANCED_FACE('',(#1444),#959,.F.);
#12054=ADVANCED_FACE('',(#1445),#960,.F.);
#12055=ADVANCED_FACE('',(#1446),#11818,.F.);
#12056=ADVANCED_FACE('',(#1447),#11819,.T.);
#12057=ADVANCED_FACE('',(#1448),#961,.F.);
#12058=ADVANCED_FACE('',(#1449),#11820,.T.);
#12059=ADVANCED_FACE('',(#1450),#962,.T.);
#12060=ADVANCED_FACE('',(#1451),#11821,.F.);
#12061=ADVANCED_FACE('',(#1452),#11822,.F.);
#12062=ADVANCED_FACE('',(#1453),#963,.F.);
#12063=ADVANCED_FACE('',(#1454),#964,.F.);
#12064=ADVANCED_FACE('',(#1455),#965,.F.);
#12065=ADVANCED_FACE('',(#1456),#966,.F.);
#12066=ADVANCED_FACE('',(#1457),#967,.T.);
#12067=ADVANCED_FACE('',(#1458),#968,.T.);
#12068=ADVANCED_FACE('',(#1459,#753,#754),#969,.T.);
#12069=ADVANCED_FACE('',(#1460),#11823,.F.);
#12070=ADVANCED_FACE('',(#1461),#970,.T.);
#12071=ADVANCED_FACE('',(#1462),#971,.T.);
#12072=ADVANCED_FACE('',(#1463),#972,.T.);
#12073=ADVANCED_FACE('',(#1464,#755,#756),#973,.F.);
#12074=ADVANCED_FACE('',(#1465),#974,.F.);
#12075=ADVANCED_FACE('',(#1466),#975,.F.);
#12076=ADVANCED_FACE('',(#1467,#757,#758),#976,.F.);
#12077=ADVANCED_FACE('',(#1468),#977,.F.);
#12078=ADVANCED_FACE('',(#1469),#978,.T.);
#12079=ADVANCED_FACE('',(#1470,#759,#760),#979,.T.);
#12080=ADVANCED_FACE('',(#1471),#980,.T.);
#12081=ADVANCED_FACE('',(#1472),#11824,.F.);
#12082=ADVANCED_FACE('',(#1473),#981,.T.);
#12083=ADVANCED_FACE('',(#1474),#11825,.F.);
#12084=ADVANCED_FACE('',(#1475,#761),#11826,.F.);
#12085=ADVANCED_FACE('',(#1476,#762),#11827,.T.);
#12086=ADVANCED_FACE('',(#1477,#763),#982,.F.);
#12087=ADVANCED_FACE('',(#1478),#11828,.F.);
#12088=ADVANCED_FACE('',(#1479),#11829,.F.);
#12089=ADVANCED_FACE('',(#1480),#11830,.F.);
#12090=ADVANCED_FACE('',(#1481),#11831,.F.);
#12091=ADVANCED_FACE('',(#1482),#11832,.F.);
#12092=ADVANCED_FACE('',(#1483),#11833,.F.);
#12093=ADVANCED_FACE('',(#1484),#11834,.F.);
#12094=ADVANCED_FACE('',(#1485,#764),#983,.T.);
#12095=ADVANCED_FACE('',(#1486,#765),#984,.T.);
#12096=ADVANCED_FACE('',(#1487),#985,.T.);
#12097=ADVANCED_FACE('',(#1488),#986,.T.);
#12098=ADVANCED_FACE('',(#1489,#766,#767,#768,#769,#770),#987,.T.);
#12099=ADVANCED_FACE('',(#1490),#988,.T.);
#12100=ADVANCED_FACE('',(#1491,#771,#772,#773,#774,#775),#989,.T.);
#12101=ADVANCED_FACE('',(#1492),#990,.T.);
#12102=ADVANCED_FACE('',(#1493),#991,.T.);
#12103=ADVANCED_FACE('',(#1494,#776,#777),#992,.F.);
#12104=ADVANCED_FACE('',(#1495),#11835,.F.);
#12105=ADVANCED_FACE('',(#1496),#11836,.F.);
#12106=ADVANCED_FACE('',(#1497),#11837,.F.);
#12107=ADVANCED_FACE('',(#1498),#11838,.F.);
#12108=ADVANCED_FACE('',(#1499),#11839,.T.);
#12109=ADVANCED_FACE('',(#1500,#778),#993,.T.);
#12110=ADVANCED_FACE('',(#1501),#11840,.F.);
#12111=ADVANCED_FACE('',(#1502),#11841,.T.);
#12112=ADVANCED_FACE('',(#1503,#779,#780,#781,#782,#783),#994,.T.);
#12113=ADVANCED_FACE('',(#1504,#784,#785,#786,#787,#788),#995,.F.);
#12114=ADVANCED_FACE('',(#1505),#11842,.F.);
#12115=ADVANCED_FACE('',(#1506),#11843,.F.);
#12116=ADVANCED_FACE('',(#1507),#11844,.F.);
#12117=ADVANCED_FACE('',(#1508),#11845,.F.);
#12118=ADVANCED_FACE('',(#1509),#11846,.T.);
#12119=ADVANCED_FACE('',(#1510,#789),#996,.F.);
#12120=ADVANCED_FACE('',(#1511),#11847,.F.);
#12121=ADVANCED_FACE('',(#1512),#11848,.T.);
#12122=ADVANCED_FACE('',(#1513,#790,#791,#792,#793,#794),#997,.T.);
#12123=ADVANCED_FACE('',(#1514,#795,#796,#797,#798,#799),#998,.F.);
#12124=ADVANCED_FACE('',(#1515),#11849,.F.);
#12125=ADVANCED_FACE('',(#1516),#11850,.F.);
#12126=ADVANCED_FACE('',(#1517),#11851,.F.);
#12127=ADVANCED_FACE('',(#1518),#11852,.F.);
#12128=ADVANCED_FACE('',(#1519),#11853,.F.);
#12129=ADVANCED_FACE('',(#1520),#11854,.F.);
#12130=ADVANCED_FACE('',(#1521),#11855,.F.);
#12131=ADVANCED_FACE('',(#1522,#800),#999,.T.);
#12132=ADVANCED_FACE('',(#1523,#801),#1000,.T.);
#12133=ADVANCED_FACE('',(#1524),#1001,.T.);
#12134=ADVANCED_FACE('',(#1525),#1002,.T.);
#12135=ADVANCED_FACE('',(#1526,#802,#803,#804,#805,#806),#1003,.T.);
#12136=ADVANCED_FACE('',(#1527),#1004,.T.);
#12137=ADVANCED_FACE('',(#1528,#807,#808,#809,#810,#811),#1005,.T.);
#12138=ADVANCED_FACE('',(#1529),#1006,.T.);
#12139=ADVANCED_FACE('',(#1530),#1007,.T.);
#12140=ADVANCED_FACE('',(#1531,#812,#813),#1008,.F.);
#12141=ADVANCED_FACE('',(#1532),#11856,.F.);
#12142=ADVANCED_FACE('',(#1533),#11857,.F.);
#12143=ADVANCED_FACE('',(#1534),#11858,.F.);
#12144=ADVANCED_FACE('',(#1535),#11859,.F.);
#12145=ADVANCED_FACE('',(#1536),#11860,.T.);
#12146=ADVANCED_FACE('',(#1537,#814),#1009,.T.);
#12147=ADVANCED_FACE('',(#1538),#11861,.F.);
#12148=ADVANCED_FACE('',(#1539),#11862,.T.);
#12149=ADVANCED_FACE('',(#1540,#815,#816,#817,#818,#819),#1010,.T.);
#12150=ADVANCED_FACE('',(#1541,#820,#821,#822,#823,#824),#1011,.F.);
#12151=ADVANCED_FACE('',(#1542),#11863,.F.);
#12152=ADVANCED_FACE('',(#1543),#11864,.F.);
#12153=ADVANCED_FACE('',(#1544),#11865,.F.);
#12154=ADVANCED_FACE('',(#1545),#11866,.F.);
#12155=ADVANCED_FACE('',(#1546),#11867,.T.);
#12156=ADVANCED_FACE('',(#1547,#825),#1012,.F.);
#12157=ADVANCED_FACE('',(#1548),#11868,.F.);
#12158=ADVANCED_FACE('',(#1549),#11869,.T.);
#12159=ADVANCED_FACE('',(#1550,#826,#827,#828,#829,#830),#1013,.T.);
#12160=ADVANCED_FACE('',(#1551,#831,#832,#833,#834,#835),#1014,.F.);
#12161=ADVANCED_FACE('',(#1552),#1015,.T.);
#12162=ADVANCED_FACE('',(#1553),#473,.T.);
#12163=ADVANCED_FACE('',(#1554),#11870,.T.);
#12164=ADVANCED_FACE('',(#1555),#1016,.F.);
#12165=ADVANCED_FACE('',(#1556),#471,.F.);
#12166=ADVANCED_FACE('',(#1557),#11871,.T.);
#12167=ADVANCED_FACE('',(#1558),#11872,.F.);
#12168=ADVANCED_FACE('',(#1559),#474,.F.);
#12169=ADVANCED_FACE('',(#1560,#836),#1017,.T.);
#12170=ADVANCED_FACE('',(#1561),#11873,.T.);
#12171=ADVANCED_FACE('',(#1562,#837),#1018,.T.);
#12172=ADVANCED_FACE('',(#1563),#475,.F.);
#12173=ADVANCED_FACE('',(#1564),#472,.F.);
#12174=ADVANCED_FACE('',(#1565),#11874,.F.);
#12175=ADVANCED_FACE('',(#1566,#838),#1019,.T.);
#12176=ADVANCED_FACE('',(#1567),#476,.T.);
#12177=ADVANCED_FACE('',(#1568),#11875,.T.);
#12178=ADVANCED_FACE('',(#1569),#477,.T.);
#12179=ADVANCED_FACE('',(#1570,#839),#1020,.T.);
#12180=ADVANCED_FACE('',(#1571),#11876,.F.);
#12181=ADVANCED_FACE('',(#1572),#457,.T.);
#12182=ADVANCED_FACE('',(#1573),#458,.T.);
#12183=ADVANCED_FACE('',(#1574),#459,.T.);
#12184=ADVANCED_FACE('',(#1575),#460,.T.);
#12185=ADVANCED_FACE('',(#1576),#461,.T.);
#12186=ADVANCED_FACE('',(#1577),#462,.T.);
#12187=ADVANCED_FACE('',(#1578),#463,.T.);
#12188=ADVANCED_FACE('',(#1579),#464,.F.);
#12189=ADVANCED_FACE('',(#1580),#11877,.T.);
#12190=ADVANCED_FACE('',(#1581),#1021,.T.);
#12191=ADVANCED_FACE('',(#1582),#465,.F.);
#12192=ADVANCED_FACE('',(#1583),#1022,.T.);
#12193=ADVANCED_FACE('',(#1584),#466,.F.);
#12194=ADVANCED_FACE('',(#1585),#1023,.T.);
#12195=ADVANCED_FACE('',(#1586),#467,.F.);
#12196=ADVANCED_FACE('',(#1587),#1024,.T.);
#12197=ADVANCED_FACE('',(#1588),#468,.F.);
#12198=ADVANCED_FACE('',(#1589),#1025,.T.);
#12199=ADVANCED_FACE('',(#1590),#469,.F.);
#12200=ADVANCED_FACE('',(#1591),#11878,.F.);
#12201=ADVANCED_FACE('',(#1592),#1026,.T.);
#12202=ADVANCED_FACE('',(#1593),#470,.F.);
#12203=ADVANCED_FACE('',(#1594,#840),#1027,.T.);
#12204=ADVANCED_FACE('',(#1595),#1028,.T.);
#12205=ADVANCED_FACE('',(#1596,#841),#1029,.T.);
#12206=ADVANCED_FACE('',(#1597),#11879,.T.);
#12207=ADVANCED_FACE('',(#1598,#842),#1030,.T.);
#12208=ADVANCED_FACE('',(#1599),#11880,.F.);
#12209=ADVANCED_FACE('',(#1600,#843),#1031,.T.);
#12210=ADVANCED_FACE('',(#1601),#11881,.T.);
#12211=ADVANCED_FACE('',(#1602,#844),#1032,.T.);
#12212=ADVANCED_FACE('',(#1603),#11882,.F.);
#12213=ADVANCED_FACE('',(#1604),#1033,.F.);
#12214=ADVANCED_FACE('',(#1605),#1034,.F.);
#12215=ADVANCED_FACE('',(#1606),#1035,.F.);
#12216=ADVANCED_FACE('',(#1607),#1036,.F.);
#12217=ADVANCED_FACE('',(#1608),#1037,.F.);
#12218=ADVANCED_FACE('',(#1609),#1038,.F.);
#12219=ADVANCED_FACE('',(#1610),#1039,.F.);
#12220=ADVANCED_FACE('',(#1611),#1040,.F.);
#12221=ADVANCED_FACE('',(#1612),#1041,.F.);
#12222=ADVANCED_FACE('',(#1613),#1042,.T.);
#12223=ADVANCED_FACE('',(#1614),#478,.T.);
#12224=ADVANCED_FACE('',(#1615),#11883,.T.);
#12225=ADVANCED_FACE('',(#1616),#479,.T.);
#12226=ADVANCED_FACE('',(#1617,#845),#1043,.T.);
#12227=ADVANCED_FACE('',(#1618),#480,.T.);
#12228=ADVANCED_FACE('',(#1619),#11884,.T.);
#12229=ADVANCED_FACE('',(#1620),#11885,.F.);
#12230=ADVANCED_FACE('',(#1621),#1044,.F.);
#12231=ADVANCED_FACE('',(#1622),#1045,.T.);
#12232=ADVANCED_FACE('',(#1623),#1046,.T.);
#12233=ADVANCED_FACE('',(#1624),#1047,.T.);
#12234=ADVANCED_FACE('',(#1625),#1048,.T.);
#12235=ADVANCED_FACE('',(#1626),#1049,.T.);
#12236=ADVANCED_FACE('',(#1627),#1050,.T.);
#12237=ADVANCED_FACE('',(#1628),#1051,.T.);
#12238=ADVANCED_FACE('',(#1629),#1052,.T.);
#12239=ADVANCED_FACE('',(#1630),#1053,.T.);
#12240=ADVANCED_FACE('',(#1631),#1054,.T.);
#12241=ADVANCED_FACE('',(#1632),#1055,.T.);
#12242=ADVANCED_FACE('',(#1633),#1056,.T.);
#12243=ADVANCED_FACE('',(#1634),#1057,.T.);
#12244=ADVANCED_FACE('',(#1635),#1058,.T.);
#12245=ADVANCED_FACE('',(#1636),#1059,.T.);
#12246=ADVANCED_FACE('',(#1637),#1060,.T.);
#12247=ADVANCED_FACE('',(#1638),#1061,.T.);
#12248=ADVANCED_FACE('',(#1639),#1062,.T.);
#12249=ADVANCED_FACE('',(#1640),#1063,.T.);
#12250=ADVANCED_FACE('',(#1641),#1064,.T.);
#12251=ADVANCED_FACE('',(#1642),#1065,.T.);
#12252=ADVANCED_FACE('',(#1643),#1066,.T.);
#12253=ADVANCED_FACE('',(#1644),#1067,.T.);
#12254=ADVANCED_FACE('',(#1645),#1068,.T.);
#12255=ADVANCED_FACE('',(#1646),#1069,.T.);
#12256=ADVANCED_FACE('',(#1647),#1070,.T.);
#12257=ADVANCED_FACE('',(#1648),#1071,.T.);
#12258=ADVANCED_FACE('',(#1649),#1072,.T.);
#12259=ADVANCED_FACE('',(#1650),#1073,.T.);
#12260=ADVANCED_FACE('',(#1651),#1074,.T.);
#12261=ADVANCED_FACE('',(#1652),#1075,.T.);
#12262=ADVANCED_FACE('',(#1653),#1076,.T.);
#12263=ADVANCED_FACE('',(#1654),#1077,.T.);
#12264=ADVANCED_FACE('',(#1655),#1078,.T.);
#12265=ADVANCED_FACE('',(#1656),#1079,.T.);
#12266=ADVANCED_FACE('',(#1657),#1080,.T.);
#12267=ADVANCED_FACE('',(#1658),#1081,.T.);
#12268=ADVANCED_FACE('',(#1659),#1082,.T.);
#12269=ADVANCED_FACE('',(#1660),#1083,.T.);
#12270=ADVANCED_FACE('',(#1661),#1084,.T.);
#12271=ADVANCED_FACE('',(#1662),#1085,.T.);
#12272=ADVANCED_FACE('',(#1663),#1086,.T.);
#12273=ADVANCED_FACE('',(#1664),#1087,.T.);
#12274=ADVANCED_FACE('',(#1665),#1088,.T.);
#12275=ADVANCED_FACE('',(#1666),#1089,.T.);
#12276=ADVANCED_FACE('',(#1667),#1090,.T.);
#12277=ADVANCED_FACE('',(#1668),#1091,.T.);
#12278=ADVANCED_FACE('',(#1669),#1092,.T.);
#12279=ADVANCED_FACE('',(#1670),#1093,.T.);
#12280=ADVANCED_FACE('',(#1671),#1094,.T.);
#12281=ADVANCED_FACE('',(#1672),#1095,.T.);
#12282=ADVANCED_FACE('',(#1673),#1096,.T.);
#12283=ADVANCED_FACE('',(#1674),#1097,.T.);
#12284=ADVANCED_FACE('',(#1675),#1098,.T.);
#12285=ADVANCED_FACE('',(#1676),#1099,.T.);
#12286=ADVANCED_FACE('',(#1677),#1100,.T.);
#12287=ADVANCED_FACE('',(#1678),#1101,.T.);
#12288=ADVANCED_FACE('',(#1679),#1102,.T.);
#12289=ADVANCED_FACE('',(#1680),#1103,.T.);
#12290=ADVANCED_FACE('',(#1681),#1104,.T.);
#12291=ADVANCED_FACE('',(#1682),#1105,.T.);
#12292=ADVANCED_FACE('',(#1683),#1106,.T.);
#12293=ADVANCED_FACE('',(#1684),#1107,.T.);
#12294=ADVANCED_FACE('',(#1685),#1108,.T.);
#12295=ADVANCED_FACE('',(#1686),#1109,.T.);
#12296=ADVANCED_FACE('',(#1687),#1110,.T.);
#12297=ADVANCED_FACE('',(#1688),#1111,.T.);
#12298=ADVANCED_FACE('',(#1689),#1112,.T.);
#12299=ADVANCED_FACE('',(#1690),#1113,.T.);
#12300=ADVANCED_FACE('',(#1691),#1114,.T.);
#12301=ADVANCED_FACE('',(#1692),#1115,.T.);
#12302=ADVANCED_FACE('',(#1693),#1116,.T.);
#12303=ADVANCED_FACE('',(#1694),#1117,.T.);
#12304=ADVANCED_FACE('',(#1695),#1118,.T.);
#12305=ADVANCED_FACE('',(#1696),#1119,.T.);
#12306=ADVANCED_FACE('',(#1697),#1120,.T.);
#12307=ADVANCED_FACE('',(#1698),#1121,.T.);
#12308=ADVANCED_FACE('',(#1699),#1122,.T.);
#12309=ADVANCED_FACE('',(#1700),#1123,.T.);
#12310=ADVANCED_FACE('',(#1701),#1124,.T.);
#12311=ADVANCED_FACE('',(#1702),#1125,.T.);
#12312=ADVANCED_FACE('',(#1703),#1126,.T.);
#12313=ADVANCED_FACE('',(#1704),#1127,.T.);
#12314=ADVANCED_FACE('',(#1705),#1128,.T.);
#12315=ADVANCED_FACE('',(#1706),#1129,.T.);
#12316=ADVANCED_FACE('',(#1707),#1130,.T.);
#12317=ADVANCED_FACE('',(#1708),#1131,.T.);
#12318=ADVANCED_FACE('',(#1709),#1132,.T.);
#12319=ADVANCED_FACE('',(#1710),#1133,.T.);
#12320=ADVANCED_FACE('',(#1711),#1134,.T.);
#12321=ADVANCED_FACE('',(#1712),#1135,.T.);
#12322=ADVANCED_FACE('',(#1713),#1136,.T.);
#12323=ADVANCED_FACE('',(#1714),#1137,.T.);
#12324=ADVANCED_FACE('',(#1715),#1138,.T.);
#12325=ADVANCED_FACE('',(#1716),#1139,.T.);
#12326=ADVANCED_FACE('',(#1717),#1140,.T.);
#12327=ADVANCED_FACE('',(#1718),#1141,.T.);
#12328=ADVANCED_FACE('',(#1719),#1142,.T.);
#12329=ADVANCED_FACE('',(#1720),#1143,.T.);
#12330=ADVANCED_FACE('',(#1721),#1144,.T.);
#12331=ADVANCED_FACE('',(#1722),#1145,.T.);
#12332=ADVANCED_FACE('',(#1723),#1146,.T.);
#12333=ADVANCED_FACE('',(#1724),#1147,.T.);
#12334=ADVANCED_FACE('',(#1725),#1148,.T.);
#12335=ADVANCED_FACE('',(#1726),#1149,.T.);
#12336=ADVANCED_FACE('',(#1727),#1150,.T.);
#12337=ADVANCED_FACE('',(#1728),#1151,.T.);
#12338=ADVANCED_FACE('',(#1729),#1152,.T.);
#12339=ADVANCED_FACE('',(#1730),#1153,.T.);
#12340=ADVANCED_FACE('',(#1731),#1154,.T.);
#12341=ADVANCED_FACE('',(#1732),#1155,.T.);
#12342=ADVANCED_FACE('',(#1733),#1156,.T.);
#12343=ADVANCED_FACE('',(#1734),#1157,.T.);
#12344=ADVANCED_FACE('',(#1735),#1158,.T.);
#12345=ADVANCED_FACE('',(#1736),#1159,.T.);
#12346=ADVANCED_FACE('',(#1737),#1160,.T.);
#12347=ADVANCED_FACE('',(#1738),#1161,.T.);
#12348=ADVANCED_FACE('',(#1739),#1162,.T.);
#12349=ADVANCED_FACE('',(#1740),#1163,.T.);
#12350=ADVANCED_FACE('',(#1741),#1164,.T.);
#12351=ADVANCED_FACE('',(#1742),#1165,.T.);
#12352=ADVANCED_FACE('',(#1743),#1166,.T.);
#12353=ADVANCED_FACE('',(#1744),#1167,.T.);
#12354=ADVANCED_FACE('',(#1745),#1168,.T.);
#12355=ADVANCED_FACE('',(#1746),#1169,.T.);
#12356=ADVANCED_FACE('',(#1747),#1170,.T.);
#12357=ADVANCED_FACE('',(#1748),#1171,.T.);
#12358=ADVANCED_FACE('',(#1749),#1172,.T.);
#12359=ADVANCED_FACE('',(#1750),#1173,.T.);
#12360=ADVANCED_FACE('',(#1751),#1174,.T.);
#12361=ADVANCED_FACE('',(#1752),#1175,.T.);
#12362=ADVANCED_FACE('',(#1753),#1176,.T.);
#12363=ADVANCED_FACE('',(#1754),#1177,.T.);
#12364=ADVANCED_FACE('',(#1755),#1178,.T.);
#12365=ADVANCED_FACE('',(#1756),#1179,.T.);
#12366=ADVANCED_FACE('',(#1757),#1180,.T.);
#12367=ADVANCED_FACE('',(#1758),#1181,.T.);
#12368=ADVANCED_FACE('',(#1759),#1182,.T.);
#12369=ADVANCED_FACE('',(#1760),#1183,.T.);
#12370=ADVANCED_FACE('',(#1761),#1184,.T.);
#12371=ADVANCED_FACE('',(#1762),#1185,.T.);
#12372=ADVANCED_FACE('',(#1763),#1186,.T.);
#12373=ADVANCED_FACE('',(#1764),#1187,.T.);
#12374=ADVANCED_FACE('',(#1765),#1188,.T.);
#12375=ADVANCED_FACE('',(#1766),#1189,.T.);
#12376=ADVANCED_FACE('',(#1767),#1190,.T.);
#12377=ADVANCED_FACE('',(#1768),#1191,.T.);
#12378=ADVANCED_FACE('',(#1769),#1192,.T.);
#12379=ADVANCED_FACE('',(#1770),#1193,.T.);
#12380=ADVANCED_FACE('',(#1771),#1194,.T.);
#12381=ADVANCED_FACE('',(#1772),#1195,.T.);
#12382=ADVANCED_FACE('',(#1773),#1196,.T.);
#12383=ADVANCED_FACE('',(#1774),#1197,.T.);
#12384=ADVANCED_FACE('',(#1775),#1198,.T.);
#12385=ADVANCED_FACE('',(#1776),#1199,.T.);
#12386=ADVANCED_FACE('',(#1777),#1200,.T.);
#12387=ADVANCED_FACE('',(#1778),#1201,.T.);
#12388=ADVANCED_FACE('',(#1779),#1202,.T.);
#12389=ADVANCED_FACE('',(#1780),#1203,.T.);
#12390=ADVANCED_FACE('',(#1781),#1204,.T.);
#12391=ADVANCED_FACE('',(#1782),#1205,.T.);
#12392=ADVANCED_FACE('',(#1783),#1206,.T.);
#12393=ADVANCED_FACE('',(#1784),#1207,.T.);
#12394=ADVANCED_FACE('',(#1785),#1208,.T.);
#12395=ADVANCED_FACE('',(#1786),#1209,.T.);
#12396=ADVANCED_FACE('',(#1787),#1210,.T.);
#12397=ADVANCED_FACE('',(#1788),#1211,.F.);
#12398=ADVANCED_FACE('',(#1789),#11886,.T.);
#12399=ADVANCED_FACE('',(#1790),#1212,.T.);
#12400=ADVANCED_FACE('',(#1791,#846),#1213,.F.);
#12401=ADVANCED_FACE('',(#1792),#1214,.T.);
#12402=ADVANCED_FACE('',(#1793),#11887,.F.);
#12403=ADVANCED_FACE('',(#1794),#1215,.T.);
#12404=ADVANCED_FACE('',(#1795,#847),#11888,.F.);
#12405=ADVANCED_FACE('',(#1796),#11889,.T.);
#12406=ADVANCED_FACE('',(#1797,#848),#1216,.T.);
#12407=ADVANCED_FACE('',(#1798,#849),#11890,.T.);
#12408=ADVANCED_FACE('',(#1799,#850),#1217,.T.);
#12409=ADVANCED_FACE('',(#1800,#851),#1218,.F.);
#12410=ADVANCED_FACE('',(#1801),#11891,.T.);
#12411=ADVANCED_FACE('',(#1802),#1219,.T.);
#12412=ADVANCED_FACE('',(#1803),#1220,.F.);
#12413=ADVANCED_FACE('',(#1804),#11892,.T.);
#12414=ADVANCED_FACE('',(#1805),#1221,.T.);
#12415=ADVANCED_FACE('',(#1806),#1222,.F.);
#12416=ADVANCED_FACE('',(#1807),#11893,.F.);
#12417=ADVANCED_FACE('',(#1808),#1223,.F.);
#12418=ADVANCED_FACE('',(#1809),#1224,.F.);
#12419=ADVANCED_FACE('',(#1810),#1225,.F.);
#12420=ADVANCED_FACE('',(#1811),#1226,.F.);
#12421=ADVANCED_FACE('',(#1812),#1227,.T.);
#12422=ADVANCED_FACE('',(#1813,#852),#11894,.T.);
#12423=ADVANCED_FACE('',(#1814,#853),#11895,.F.);
#12424=ADVANCED_FACE('',(#1815),#1228,.F.);
#12425=ADVANCED_FACE('',(#1816),#1229,.F.);
#12426=ADVANCED_FACE('',(#1817),#1230,.F.);
#12427=ADVANCED_FACE('',(#1818),#1231,.F.);
#12428=ADVANCED_FACE('',(#1819),#1232,.F.);
#12429=ADVANCED_FACE('',(#1820),#1233,.F.);
#12430=ADVANCED_FACE('',(#1821),#1234,.F.);
#12431=ADVANCED_FACE('',(#1822),#1235,.F.);
#12432=ADVANCED_FACE('',(#1823,#854),#1236,.T.);
#12433=ADVANCED_FACE('',(#1824),#481,.T.);
#12434=ADVANCED_FACE('',(#1825),#11896,.T.);
#12435=ADVANCED_FACE('',(#1826),#482,.T.);
#12436=ADVANCED_FACE('',(#1827),#1237,.T.);
#12437=ADVANCED_FACE('',(#1828),#11897,.F.);
#12438=ADVANCED_FACE('',(#1829),#1238,.T.);
#12439=ADVANCED_FACE('',(#1830),#11898,.F.);
#12440=ADVANCED_FACE('',(#1831),#1239,.F.);
#12441=ADVANCED_FACE('',(#1832),#1240,.F.);
#12442=ADVANCED_FACE('',(#1833),#1241,.T.);
#12443=ADVANCED_FACE('',(#1834),#1242,.F.);
#12444=ADVANCED_FACE('',(#1835),#1243,.F.);
#12445=ADVANCED_FACE('',(#1836),#1244,.F.);
#12446=ADVANCED_FACE('',(#1837),#1245,.F.);
#12447=ADVANCED_FACE('',(#1838),#1246,.T.);
#12448=ADVANCED_FACE('',(#1839),#1247,.F.);
#12449=ADVANCED_FACE('',(#1840),#1248,.F.);
#12450=ADVANCED_FACE('',(#1841),#1249,.F.);
#12451=ADVANCED_FACE('',(#1842,#855,#856),#11899,.T.);
#12452=ADVANCED_FACE('',(#1843,#857),#1250,.T.);
#12453=ADVANCED_FACE('',(#1844,#858),#1251,.F.);
#12454=ADVANCED_FACE('',(#1845),#11900,.F.);
#12455=ADVANCED_FACE('',(#1846),#11901,.T.);
#12456=ADVANCED_FACE('',(#1847,#859),#1252,.T.);
#12457=ADVANCED_FACE('',(#1848,#860),#1253,.F.);
#12458=ADVANCED_FACE('',(#1849),#11902,.F.);
#12459=ADVANCED_FACE('',(#1850),#11903,.T.);
#12460=ADVANCED_FACE('',(#1851,#861),#1254,.T.);
#12461=ADVANCED_FACE('',(#1852,#862),#1255,.F.);
#12462=ADVANCED_FACE('',(#1853),#11904,.F.);
#12463=ADVANCED_FACE('',(#1854),#11905,.T.);
#12464=ADVANCED_FACE('',(#1855,#863),#1256,.T.);
#12465=ADVANCED_FACE('',(#1856,#864),#1257,.F.);
#12466=ADVANCED_FACE('',(#1857),#11906,.F.);
#12467=ADVANCED_FACE('',(#1858),#11907,.T.);
#12468=ADVANCED_FACE('',(#1859,#865),#1258,.T.);
#12469=ADVANCED_FACE('',(#1860,#866),#1259,.F.);
#12470=ADVANCED_FACE('',(#1861),#1260,.T.);
#12471=ADVANCED_FACE('',(#1862),#1261,.T.);
#12472=ADVANCED_FACE('',(#1863),#1262,.T.);
#12473=ADVANCED_FACE('',(#1864),#1263,.T.);
#12474=ADVANCED_FACE('',(#1865),#1264,.T.);
#12475=ADVANCED_FACE('',(#1866),#1265,.F.);
#12476=ADVANCED_FACE('',(#1867),#1266,.T.);
#12477=ADVANCED_FACE('',(#1868),#1267,.T.);
#12478=ADVANCED_FACE('',(#1869),#1268,.T.);
#12479=ADVANCED_FACE('',(#1870),#1269,.T.);
#12480=ADVANCED_FACE('',(#1871),#1270,.T.);
#12481=ADVANCED_FACE('',(#1872),#1271,.F.);
#12482=ADVANCED_FACE('',(#1873),#11908,.F.);
#12483=ADVANCED_FACE('',(#1874),#1272,.F.);
#12484=ADVANCED_FACE('',(#1875),#1273,.F.);
#12485=ADVANCED_FACE('',(#1876),#1274,.F.);
#12486=ADVANCED_FACE('',(#1877,#867),#1275,.T.);
#12487=ADVANCED_FACE('',(#1878),#11909,.F.);
#12488=ADVANCED_FACE('',(#1879),#11910,.T.);
#12489=ADVANCED_FACE('',(#1880),#1276,.T.);
#12490=ADVANCED_FACE('',(#1881,#868),#1277,.F.);
#12491=ADVANCED_FACE('',(#1882),#1278,.T.);
#12492=ADVANCED_FACE('',(#1883,#869),#1279,.T.);
#12493=ADVANCED_FACE('',(#1884,#870),#11911,.T.);
#12494=ADVANCED_FACE('',(#1885,#871),#1280,.F.);
#12495=ADVANCED_FACE('',(#1886),#11912,.F.);
#12496=ADVANCED_FACE('',(#1887),#11913,.T.);
#12497=ADVANCED_FACE('',(#1888,#872),#1281,.T.);
#12498=ADVANCED_FACE('',(#1889,#873),#1282,.F.);
#12499=ADVANCED_FACE('',(#1890),#11914,.F.);
#12500=ADVANCED_FACE('',(#1891),#11915,.T.);
#12501=ADVANCED_FACE('',(#1892,#874),#1283,.T.);
#12502=ADVANCED_FACE('',(#1893,#875),#1284,.F.);
#12503=ADVANCED_FACE('',(#1894),#11916,.F.);
#12504=ADVANCED_FACE('',(#1895),#11917,.T.);
#12505=ADVANCED_FACE('',(#1896,#876),#1285,.T.);
#12506=ADVANCED_FACE('',(#1897,#877),#1286,.F.);
#12507=ADVANCED_FACE('',(#1898),#1287,.F.);
#12508=ADVANCED_FACE('',(#1899),#1288,.F.);
#12509=ADVANCED_FACE('',(#1900),#1289,.F.);
#12510=ADVANCED_FACE('',(#1901,#878),#1290,.F.);
#12511=ADVANCED_FACE('',(#1902),#11918,.F.);
#12512=ADVANCED_FACE('',(#1903),#11919,.T.);
#12513=ADVANCED_FACE('',(#1904,#879),#1291,.T.);
#12514=ADVANCED_FACE('',(#1905),#11,.T.);
#12515=ADVANCED_FACE('',(#1906),#1292,.T.);
#12516=ADVANCED_FACE('',(#1907),#12,.T.);
#12517=ADVANCED_FACE('',(#1908),#11920,.T.);
#12518=ADVANCED_FACE('',(#1909),#13,.T.);
#12519=ADVANCED_FACE('',(#1910),#1293,.T.);
#12520=ADVANCED_FACE('',(#1911),#14,.T.);
#12521=ADVANCED_FACE('',(#1912),#11921,.T.);
#12522=ADVANCED_FACE('',(#1913),#15,.T.);
#12523=ADVANCED_FACE('',(#1914),#1294,.T.);
#12524=ADVANCED_FACE('',(#1915),#16,.T.);
#12525=ADVANCED_FACE('',(#1916),#11922,.T.);
#12526=ADVANCED_FACE('',(#1917),#17,.T.);
#12527=ADVANCED_FACE('',(#1918),#1295,.T.);
#12528=ADVANCED_FACE('',(#1919),#18,.T.);
#12529=ADVANCED_FACE('',(#1920),#11923,.T.);
#12530=ADVANCED_FACE('',(#1921),#19,.T.);
#12531=ADVANCED_FACE('',(#1922),#1296,.T.);
#12532=ADVANCED_FACE('',(#1923),#20,.T.);
#12533=ADVANCED_FACE('',(#1924),#11924,.T.);
#12534=ADVANCED_FACE('',(#1925),#21,.T.);
#12535=ADVANCED_FACE('',(#1926),#1297,.T.);
#12536=ADVANCED_FACE('',(#1927),#22,.T.);
#12537=ADVANCED_FACE('',(#1928),#11925,.T.);
#12538=ADVANCED_FACE('',(#1929),#23,.T.);
#12539=ADVANCED_FACE('',(#1930),#1298,.T.);
#12540=ADVANCED_FACE('',(#1931),#24,.T.);
#12541=ADVANCED_FACE('',(#1932),#11926,.T.);
#12542=ADVANCED_FACE('',(#1933),#25,.T.);
#12543=ADVANCED_FACE('',(#1934),#1299,.T.);
#12544=ADVANCED_FACE('',(#1935),#26,.T.);
#12545=ADVANCED_FACE('',(#1936),#11927,.T.);
#12546=ADVANCED_FACE('',(#1937),#27,.T.);
#12547=ADVANCED_FACE('',(#1938),#1300,.T.);
#12548=ADVANCED_FACE('',(#1939),#28,.T.);
#12549=ADVANCED_FACE('',(#1940),#11928,.T.);
#12550=ADVANCED_FACE('',(#1941),#29,.T.);
#12551=ADVANCED_FACE('',(#1942),#1301,.T.);
#12552=ADVANCED_FACE('',(#1943),#30,.T.);
#12553=ADVANCED_FACE('',(#1944),#11929,.T.);
#12554=ADVANCED_FACE('',(#1945),#31,.T.);
#12555=ADVANCED_FACE('',(#1946),#1302,.T.);
#12556=ADVANCED_FACE('',(#1947),#32,.T.);
#12557=ADVANCED_FACE('',(#1948),#11930,.T.);
#12558=ADVANCED_FACE('',(#1949),#33,.T.);
#12559=ADVANCED_FACE('',(#1950),#1303,.T.);
#12560=ADVANCED_FACE('',(#1951),#34,.T.);
#12561=ADVANCED_FACE('',(#1952),#11931,.T.);
#12562=ADVANCED_FACE('',(#1953),#35,.T.);
#12563=ADVANCED_FACE('',(#1954),#1304,.T.);
#12564=ADVANCED_FACE('',(#1955),#36,.T.);
#12565=ADVANCED_FACE('',(#1956),#11932,.T.);
#12566=ADVANCED_FACE('',(#1957),#37,.T.);
#12567=ADVANCED_FACE('',(#1958),#1305,.T.);
#12568=ADVANCED_FACE('',(#1959),#38,.T.);
#12569=ADVANCED_FACE('',(#1960),#11933,.T.);
#12570=ADVANCED_FACE('',(#1961),#39,.T.);
#12571=ADVANCED_FACE('',(#1962),#1306,.T.);
#12572=ADVANCED_FACE('',(#1963),#40,.T.);
#12573=ADVANCED_FACE('',(#1964),#11934,.T.);
#12574=ADVANCED_FACE('',(#1965),#41,.T.);
#12575=ADVANCED_FACE('',(#1966),#1307,.T.);
#12576=ADVANCED_FACE('',(#1967),#42,.T.);
#12577=ADVANCED_FACE('',(#1968),#11935,.T.);
#12578=ADVANCED_FACE('',(#1969),#43,.T.);
#12579=ADVANCED_FACE('',(#1970),#1308,.T.);
#12580=ADVANCED_FACE('',(#1971),#44,.T.);
#12581=ADVANCED_FACE('',(#1972),#11936,.T.);
#12582=ADVANCED_FACE('',(#1973),#45,.T.);
#12583=ADVANCED_FACE('',(#1974),#1309,.T.);
#12584=ADVANCED_FACE('',(#1975),#46,.T.);
#12585=ADVANCED_FACE('',(#1976),#11937,.T.);
#12586=ADVANCED_FACE('',(#1977),#47,.T.);
#12587=ADVANCED_FACE('',(#1978),#1310,.T.);
#12588=ADVANCED_FACE('',(#1979),#48,.T.);
#12589=ADVANCED_FACE('',(#1980),#11938,.T.);
#12590=ADVANCED_FACE('',(#1981),#49,.T.);
#12591=ADVANCED_FACE('',(#1982),#1311,.T.);
#12592=ADVANCED_FACE('',(#1983),#50,.T.);
#12593=ADVANCED_FACE('',(#1984,#880),#1312,.T.);
#12594=ADVANCED_FACE('',(#1985),#11939,.T.);
#12595=ADVANCED_FACE('',(#1986),#11940,.F.);
#12596=ADVANCED_FACE('',(#1987),#11941,.T.);
#12597=ADVANCED_FACE('',(#1988,#881),#1313,.T.);
#12598=ADVANCED_FACE('',(#1989,#882),#1314,.F.);
#12599=ADVANCED_FACE('',(#1990),#1315,.T.);
#12600=ADVANCED_FACE('',(#1991),#483,.T.);
#12601=ADVANCED_FACE('',(#1992),#11942,.T.);
#12602=ADVANCED_FACE('',(#1993),#484,.T.);
#12603=ADVANCED_FACE('',(#1994,#883),#1316,.T.);
#12604=ADVANCED_FACE('',(#1995),#485,.T.);
#12605=ADVANCED_FACE('',(#1996),#11943,.T.);
#12606=ADVANCED_FACE('',(#1997),#486,.T.);
#12607=ADVANCED_FACE('',(#1998),#1317,.T.);
#12608=ADVANCED_FACE('',(#1999),#1318,.F.);
#12609=ADVANCED_FACE('',(#2000),#1319,.F.);
#12610=ADVANCED_FACE('',(#2001),#1320,.F.);
#12611=ADVANCED_FACE('',(#2002),#1321,.F.);
#12612=ADVANCED_FACE('',(#2003),#1322,.F.);
#12613=ADVANCED_FACE('',(#2004),#1323,.F.);
#12614=ADVANCED_FACE('',(#2005),#1324,.F.);
#12615=ADVANCED_FACE('',(#2006),#1325,.F.);
#12616=ADVANCED_FACE('',(#2007),#1326,.T.);
#12617=ADVANCED_FACE('',(#2008),#487,.T.);
#12618=ADVANCED_FACE('',(#2009),#11944,.T.);
#12619=ADVANCED_FACE('',(#2010),#488,.T.);
#12620=ADVANCED_FACE('',(#2011,#884),#1327,.T.);
#12621=ADVANCED_FACE('',(#2012),#489,.T.);
#12622=ADVANCED_FACE('',(#2013),#11945,.T.);
#12623=ADVANCED_FACE('',(#2014),#490,.T.);
#12624=ADVANCED_FACE('',(#2015),#1328,.T.);
#12625=ADVANCED_FACE('',(#2016),#1329,.F.);
#12626=ADVANCED_FACE('',(#2017),#1330,.F.);
#12627=ADVANCED_FACE('',(#2018),#1331,.F.);
#12628=ADVANCED_FACE('',(#2019),#1332,.F.);
#12629=ADVANCED_FACE('',(#2020),#1333,.F.);
#12630=ADVANCED_FACE('',(#2021),#1334,.F.);
#12631=ADVANCED_FACE('',(#2022),#1335,.F.);
#12632=ADVANCED_FACE('',(#2023),#1336,.F.);
#12633=ADVANCED_FACE('',(#2024),#11946,.F.);
#12634=ADVANCED_FACE('',(#2025),#11947,.T.);
#12635=ADVANCED_FACE('',(#2026,#885),#1337,.T.);
#12636=ADVANCED_FACE('',(#2027,#886),#1338,.F.);
#12637=CLOSED_SHELL('',(#11948,#11949,#11950,#11951,#11952,#11953,#11954,
#11955,#11956,#11957,#11958,#11959));
#12638=CLOSED_SHELL('',(#11960,#11961,#11962,#11963,#11964,#11965));
#12639=CLOSED_SHELL('',(#11966,#11967,#11968,#11969,#11970,#11971));
#12640=CLOSED_SHELL('',(#11972,#11973,#11974,#11975,#11976,#11977,#11978,
#11979,#11980,#11981,#11982,#11983,#11984,#11985,#11986,#11987,#11988,#11989,
#11990,#11991,#11992,#11993,#11994,#11995,#11996,#11997,#11998,#11999,#12000,
#12001,#12002,#12003,#12004,#12005,#12006,#12007,#12008,#12009,#12010));
#12641=CLOSED_SHELL('',(#12011,#12012,#12013,#12014,#12015,#12016,#12017,
#12018,#12019,#12020,#12021,#12022,#12023,#12024,#12025));
#12642=CLOSED_SHELL('',(#12026,#12027,#12028,#12029,#12030,#12031,#12032,
#12033,#12034,#12035));
#12643=CLOSED_SHELL('',(#12036,#12037,#12038,#12039,#12040,#12041,#12042,
#12043,#12044,#12045,#12046,#12047,#12048,#12049));
#12644=CLOSED_SHELL('',(#12050,#12051,#12052,#12053,#12054,#12055,#12056,
#12057,#12058,#12059));
#12645=CLOSED_SHELL('',(#12060,#12061,#12062,#12063,#12064,#12065,#12066,
#12067,#12068,#12069,#12070,#12071,#12072,#12073));
#12646=CLOSED_SHELL('',(#12074,#12075,#12076,#12077,#12078,#12079,#12080,
#12081,#12082,#12083,#12084,#12085,#12086));
#12647=CLOSED_SHELL('',(#12087,#12088,#12089,#12090,#12091,#12092,#12093,
#12094,#12095,#12096,#12097,#12098,#12099,#12100,#12101,#12102,#12103));
#12648=CLOSED_SHELL('',(#12104,#12105,#12106,#12107,#12108,#12109,#12110,
#12111,#12112,#12113));
#12649=CLOSED_SHELL('',(#12114,#12115,#12116,#12117,#12118,#12119,#12120,
#12121,#12122,#12123));
#12650=CLOSED_SHELL('',(#12124,#12125,#12126,#12127,#12128,#12129,#12130,
#12131,#12132,#12133,#12134,#12135,#12136,#12137,#12138,#12139,#12140));
#12651=CLOSED_SHELL('',(#12141,#12142,#12143,#12144,#12145,#12146,#12147,
#12148,#12149,#12150));
#12652=CLOSED_SHELL('',(#12151,#12152,#12153,#12154,#12155,#12156,#12157,
#12158,#12159,#12160));
#12653=CLOSED_SHELL('',(#12161,#12162,#12163,#12164));
#12654=CLOSED_SHELL('',(#12165,#12166,#12167,#12168,#12169,#12170,#12171,
#12172));
#12655=CLOSED_SHELL('',(#12173,#12174,#12175,#12176,#12177,#12178,#12179,
#12180));
#12656=CLOSED_SHELL('',(#12181));
#12657=CLOSED_SHELL('',(#12182));
#12658=CLOSED_SHELL('',(#12183));
#12659=CLOSED_SHELL('',(#12184));
#12660=CLOSED_SHELL('',(#12185));
#12661=CLOSED_SHELL('',(#12186));
#12662=CLOSED_SHELL('',(#12187));
#12663=CLOSED_SHELL('',(#12188,#12189,#12190,#12191,#12192,#12193,#12194,
#12195,#12196,#12197,#12198,#12199,#12200,#12201,#12202,#12203,#12204));
#12664=CLOSED_SHELL('',(#12205,#12206,#12207,#12208));
#12665=CLOSED_SHELL('',(#12209,#12210,#12211,#12212));
#12666=CLOSED_SHELL('',(#12213,#12214,#12215,#12216,#12217,#12218,#12219,
#12220));
#12667=CLOSED_SHELL('',(#12221,#12222,#12223,#12224,#12225,#12226,#12227,
#12228));
#12668=CLOSED_SHELL('',(#12229,#12230,#12231,#12232,#12233,#12234,#12235,
#12236,#12237,#12238,#12239,#12240,#12241,#12242,#12243,#12244,#12245,#12246,
#12247,#12248,#12249,#12250,#12251,#12252,#12253,#12254,#12255,#12256,#12257,
#12258,#12259,#12260,#12261,#12262,#12263,#12264,#12265,#12266,#12267,#12268,
#12269,#12270,#12271,#12272,#12273,#12274,#12275,#12276,#12277,#12278,#12279,
#12280,#12281,#12282,#12283,#12284,#12285,#12286,#12287,#12288,#12289,#12290,
#12291,#12292,#12293,#12294,#12295,#12296,#12297,#12298,#12299,#12300,#12301,
#12302,#12303,#12304,#12305,#12306,#12307,#12308,#12309,#12310,#12311,#12312,
#12313,#12314,#12315,#12316,#12317,#12318,#12319,#12320,#12321,#12322,#12323,
#12324,#12325,#12326,#12327,#12328,#12329,#12330,#12331,#12332,#12333,#12334,
#12335,#12336,#12337,#12338,#12339,#12340,#12341,#12342,#12343,#12344,#12345,
#12346,#12347,#12348,#12349,#12350,#12351,#12352,#12353,#12354,#12355,#12356,
#12357,#12358,#12359,#12360,#12361,#12362,#12363,#12364,#12365,#12366,#12367,
#12368,#12369,#12370,#12371,#12372,#12373,#12374,#12375,#12376,#12377,#12378,
#12379,#12380,#12381,#12382,#12383,#12384,#12385,#12386,#12387,#12388,#12389,
#12390,#12391,#12392,#12393,#12394,#12395,#12396,#12397,#12398,#12399,#12400));
#12669=CLOSED_SHELL('',(#12401,#12402,#12403,#12404,#12405,#12406,#12407,
#12408,#12409));
#12670=CLOSED_SHELL('',(#12410,#12411,#12412));
#12671=CLOSED_SHELL('',(#12413,#12414,#12415));
#12672=CLOSED_SHELL('',(#12416,#12417,#12418,#12419,#12420,#12421,#12422,
#12423,#12424));
#12673=CLOSED_SHELL('',(#12425,#12426,#12427,#12428,#12429,#12430,#12431,
#12432,#12433,#12434,#12435,#12436));
#12674=CLOSED_SHELL('',(#12437,#12438,#12439,#12440,#12441,#12442,#12443,
#12444,#12445,#12446,#12447,#12448,#12449,#12450,#12451,#12452,#12453));
#12675=CLOSED_SHELL('',(#12454,#12455,#12456,#12457));
#12676=CLOSED_SHELL('',(#12458,#12459,#12460,#12461));
#12677=CLOSED_SHELL('',(#12462,#12463,#12464,#12465));
#12678=CLOSED_SHELL('',(#12466,#12467,#12468,#12469));
#12679=CLOSED_SHELL('',(#12470,#12471,#12472,#12473,#12474,#12475));
#12680=CLOSED_SHELL('',(#12476,#12477,#12478,#12479,#12480,#12481));
#12681=CLOSED_SHELL('',(#12482,#12483,#12484,#12485,#12486,#12487,#12488,
#12489,#12490,#12491,#12492,#12493,#12494));
#12682=CLOSED_SHELL('',(#12495,#12496,#12497,#12498));
#12683=CLOSED_SHELL('',(#12499,#12500,#12501,#12502));
#12684=CLOSED_SHELL('',(#12503,#12504,#12505,#12506));
#12685=CLOSED_SHELL('',(#12507,#12508,#12509,#12510,#12511,#12512,#12513,
#12514,#12515,#12516,#12517,#12518,#12519,#12520,#12521,#12522,#12523,#12524,
#12525,#12526,#12527,#12528,#12529,#12530,#12531,#12532,#12533,#12534,#12535,
#12536,#12537,#12538,#12539,#12540,#12541,#12542,#12543,#12544,#12545,#12546,
#12547,#12548,#12549,#12550,#12551,#12552,#12553,#12554,#12555,#12556,#12557,
#12558,#12559,#12560,#12561,#12562,#12563,#12564,#12565,#12566,#12567,#12568,
#12569,#12570,#12571,#12572,#12573,#12574,#12575,#12576,#12577,#12578,#12579,
#12580,#12581,#12582,#12583,#12584,#12585,#12586,#12587,#12588,#12589,#12590,
#12591,#12592,#12593,#12594));
#12686=CLOSED_SHELL('',(#12595,#12596,#12597,#12598));
#12687=CLOSED_SHELL('',(#12599,#12600,#12601,#12602,#12603,#12604,#12605,
#12606,#12607));
#12688=CLOSED_SHELL('',(#12608,#12609,#12610,#12611,#12612,#12613,#12614,
#12615));
#12689=CLOSED_SHELL('',(#12616,#12617,#12618,#12619,#12620,#12621,#12622,
#12623,#12624));
#12690=CLOSED_SHELL('',(#12625,#12626,#12627,#12628,#12629,#12630,#12631,
#12632));
#12691=CLOSED_SHELL('',(#12633,#12634,#12635,#12636));
#12692=DERIVED_UNIT_ELEMENT(#12782,1.);
#12693=DERIVED_UNIT_ELEMENT(#33301,-3.);
#12694=DERIVED_UNIT_ELEMENT(#12782,1.);
#12695=DERIVED_UNIT_ELEMENT(#33301,-3.);
#12696=DERIVED_UNIT_ELEMENT(#12782,1.);
#12697=DERIVED_UNIT_ELEMENT(#33301,-3.);
#12698=DERIVED_UNIT_ELEMENT(#12782,1.);
#12699=DERIVED_UNIT_ELEMENT(#33301,-3.);
#12700=DERIVED_UNIT_ELEMENT(#12782,1.);
#12701=DERIVED_UNIT_ELEMENT(#33301,-3.);
#12702=DERIVED_UNIT_ELEMENT(#12782,1.);
#12703=DERIVED_UNIT_ELEMENT(#33301,-3.);
#12704=DERIVED_UNIT_ELEMENT(#12782,1.);
#12705=DERIVED_UNIT_ELEMENT(#33301,-3.);
#12706=DERIVED_UNIT_ELEMENT(#12782,1.);
#12707=DERIVED_UNIT_ELEMENT(#33301,-3.);
#12708=DERIVED_UNIT_ELEMENT(#12782,1.);
#12709=DERIVED_UNIT_ELEMENT(#33301,-3.);
#12710=DERIVED_UNIT_ELEMENT(#12782,1.);
#12711=DERIVED_UNIT_ELEMENT(#33301,-3.);
#12712=DERIVED_UNIT_ELEMENT(#12782,1.);
#12713=DERIVED_UNIT_ELEMENT(#33301,-3.);
#12714=DERIVED_UNIT_ELEMENT(#12782,1.);
#12715=DERIVED_UNIT_ELEMENT(#33301,-3.);
#12716=DERIVED_UNIT_ELEMENT(#12782,1.);
#12717=DERIVED_UNIT_ELEMENT(#33301,-3.);
#12718=DERIVED_UNIT_ELEMENT(#12782,1.);
#12719=DERIVED_UNIT_ELEMENT(#33301,-3.);
#12720=DERIVED_UNIT_ELEMENT(#12782,1.);
#12721=DERIVED_UNIT_ELEMENT(#33301,-3.);
#12722=DERIVED_UNIT_ELEMENT(#12782,1.);
#12723=DERIVED_UNIT_ELEMENT(#33301,-3.);
#12724=DERIVED_UNIT_ELEMENT(#12782,1.);
#12725=DERIVED_UNIT_ELEMENT(#33301,-3.);
#12726=DERIVED_UNIT_ELEMENT(#12782,1.);
#12727=DERIVED_UNIT_ELEMENT(#33301,-3.);
#12728=DERIVED_UNIT_ELEMENT(#12782,1.);
#12729=DERIVED_UNIT_ELEMENT(#33301,-3.);
#12730=DERIVED_UNIT_ELEMENT(#12782,1.);
#12731=DERIVED_UNIT_ELEMENT(#33301,-3.);
#12732=DERIVED_UNIT_ELEMENT(#12782,1.);
#12733=DERIVED_UNIT_ELEMENT(#33301,-3.);
#12734=DERIVED_UNIT_ELEMENT(#12782,1.);
#12735=DERIVED_UNIT_ELEMENT(#33301,-3.);
#12736=DERIVED_UNIT_ELEMENT(#12782,1.);
#12737=DERIVED_UNIT_ELEMENT(#33301,-3.);
#12738=DERIVED_UNIT_ELEMENT(#12782,1.);
#12739=DERIVED_UNIT_ELEMENT(#33301,-3.);
#12740=DERIVED_UNIT_ELEMENT(#12782,1.);
#12741=DERIVED_UNIT_ELEMENT(#33301,-3.);
#12742=DERIVED_UNIT_ELEMENT(#12782,1.);
#12743=DERIVED_UNIT_ELEMENT(#33301,-3.);
#12744=DERIVED_UNIT_ELEMENT(#12782,1.);
#12745=DERIVED_UNIT_ELEMENT(#33301,-3.);
#12746=DERIVED_UNIT_ELEMENT(#12782,1.);
#12747=DERIVED_UNIT_ELEMENT(#33301,-3.);
#12748=DERIVED_UNIT_ELEMENT(#12782,1.);
#12749=DERIVED_UNIT_ELEMENT(#33301,-3.);
#12750=DERIVED_UNIT_ELEMENT(#12782,1.);
#12751=DERIVED_UNIT_ELEMENT(#33301,-3.);
#12752=DERIVED_UNIT_ELEMENT(#12782,1.);
#12753=DERIVED_UNIT_ELEMENT(#33301,-3.);
#12754=DERIVED_UNIT_ELEMENT(#12782,1.);
#12755=DERIVED_UNIT_ELEMENT(#33301,-3.);
#12756=DERIVED_UNIT_ELEMENT(#12782,1.);
#12757=DERIVED_UNIT_ELEMENT(#33301,-3.);
#12758=DERIVED_UNIT_ELEMENT(#12782,1.);
#12759=DERIVED_UNIT_ELEMENT(#33301,-3.);
#12760=DERIVED_UNIT_ELEMENT(#12782,1.);
#12761=DERIVED_UNIT_ELEMENT(#33301,-3.);
#12762=DERIVED_UNIT_ELEMENT(#12782,1.);
#12763=DERIVED_UNIT_ELEMENT(#33301,-3.);
#12764=DERIVED_UNIT_ELEMENT(#12782,1.);
#12765=DERIVED_UNIT_ELEMENT(#33301,-3.);
#12766=DERIVED_UNIT_ELEMENT(#12782,1.);
#12767=DERIVED_UNIT_ELEMENT(#33301,-3.);
#12768=DERIVED_UNIT_ELEMENT(#12782,1.);
#12769=DERIVED_UNIT_ELEMENT(#33301,-3.);
#12770=DERIVED_UNIT_ELEMENT(#12782,1.);
#12771=DERIVED_UNIT_ELEMENT(#33301,-3.);
#12772=DERIVED_UNIT_ELEMENT(#12782,1.);
#12773=DERIVED_UNIT_ELEMENT(#33301,-3.);
#12774=DERIVED_UNIT_ELEMENT(#12782,1.);
#12775=DERIVED_UNIT_ELEMENT(#33301,-3.);
#12776=DERIVED_UNIT_ELEMENT(#12782,1.);
#12777=DERIVED_UNIT_ELEMENT(#33301,-3.);
#12778=DERIVED_UNIT_ELEMENT(#12782,1.);
#12779=DERIVED_UNIT_ELEMENT(#33301,-3.);
#12780=DERIVED_UNIT_ELEMENT(#12782,1.);
#12781=DERIVED_UNIT_ELEMENT(#33301,-3.);
#12782=(
MASS_UNIT()
NAMED_UNIT(*)
SI_UNIT(.KILO.,.GRAM.)
);
#12783=DERIVED_UNIT((#12692,#12693));
#12784=DERIVED_UNIT((#12694,#12695));
#12785=DERIVED_UNIT((#12696,#12697));
#12786=DERIVED_UNIT((#12698,#12699));
#12787=DERIVED_UNIT((#12700,#12701));
#12788=DERIVED_UNIT((#12702,#12703));
#12789=DERIVED_UNIT((#12704,#12705));
#12790=DERIVED_UNIT((#12706,#12707));
#12791=DERIVED_UNIT((#12708,#12709));
#12792=DERIVED_UNIT((#12710,#12711));
#12793=DERIVED_UNIT((#12712,#12713));
#12794=DERIVED_UNIT((#12714,#12715));
#12795=DERIVED_UNIT((#12716,#12717));
#12796=DERIVED_UNIT((#12718,#12719));
#12797=DERIVED_UNIT((#12720,#12721));
#12798=DERIVED_UNIT((#12722,#12723));
#12799=DERIVED_UNIT((#12724,#12725));
#12800=DERIVED_UNIT((#12726,#12727));
#12801=DERIVED_UNIT((#12728,#12729));
#12802=DERIVED_UNIT((#12730,#12731));
#12803=DERIVED_UNIT((#12732,#12733));
#12804=DERIVED_UNIT((#12734,#12735));
#12805=DERIVED_UNIT((#12736,#12737));
#12806=DERIVED_UNIT((#12738,#12739));
#12807=DERIVED_UNIT((#12740,#12741));
#12808=DERIVED_UNIT((#12742,#12743));
#12809=DERIVED_UNIT((#12744,#12745));
#12810=DERIVED_UNIT((#12746,#12747));
#12811=DERIVED_UNIT((#12748,#12749));
#12812=DERIVED_UNIT((#12750,#12751));
#12813=DERIVED_UNIT((#12752,#12753));
#12814=DERIVED_UNIT((#12754,#12755));
#12815=DERIVED_UNIT((#12756,#12757));
#12816=DERIVED_UNIT((#12758,#12759));
#12817=DERIVED_UNIT((#12760,#12761));
#12818=DERIVED_UNIT((#12762,#12763));
#12819=DERIVED_UNIT((#12764,#12765));
#12820=DERIVED_UNIT((#12766,#12767));
#12821=DERIVED_UNIT((#12768,#12769));
#12822=DERIVED_UNIT((#12770,#12771));
#12823=DERIVED_UNIT((#12772,#12773));
#12824=DERIVED_UNIT((#12774,#12775));
#12825=DERIVED_UNIT((#12776,#12777));
#12826=DERIVED_UNIT((#12778,#12779));
#12827=DERIVED_UNIT((#12780,#12781));
#12828=MEASURE_REPRESENTATION_ITEM('density measure',
POSITIVE_RATIO_MEASURE(7850.),#12783);
#12829=MEASURE_REPRESENTATION_ITEM('density measure',
POSITIVE_RATIO_MEASURE(7850.),#12784);
#12830=MEASURE_REPRESENTATION_ITEM('density measure',
POSITIVE_RATIO_MEASURE(7850.),#12785);
#12831=MEASURE_REPRESENTATION_ITEM('density measure',
POSITIVE_RATIO_MEASURE(7850.),#12786);
#12832=MEASURE_REPRESENTATION_ITEM('density measure',
POSITIVE_RATIO_MEASURE(7850.),#12787);
#12833=MEASURE_REPRESENTATION_ITEM('density measure',
POSITIVE_RATIO_MEASURE(7850.),#12788);
#12834=MEASURE_REPRESENTATION_ITEM('density measure',
POSITIVE_RATIO_MEASURE(7850.),#12789);
#12835=MEASURE_REPRESENTATION_ITEM('density measure',
POSITIVE_RATIO_MEASURE(7850.),#12790);
#12836=MEASURE_REPRESENTATION_ITEM('density measure',
POSITIVE_RATIO_MEASURE(7850.),#12791);
#12837=MEASURE_REPRESENTATION_ITEM('density measure',
POSITIVE_RATIO_MEASURE(7850.),#12792);
#12838=MEASURE_REPRESENTATION_ITEM('density measure',
POSITIVE_RATIO_MEASURE(7850.),#12793);
#12839=MEASURE_REPRESENTATION_ITEM('density measure',
POSITIVE_RATIO_MEASURE(7850.),#12794);
#12840=MEASURE_REPRESENTATION_ITEM('density measure',
POSITIVE_RATIO_MEASURE(7850.),#12795);
#12841=MEASURE_REPRESENTATION_ITEM('density measure',
POSITIVE_RATIO_MEASURE(7850.),#12796);
#12842=MEASURE_REPRESENTATION_ITEM('density measure',
POSITIVE_RATIO_MEASURE(7850.),#12797);
#12843=MEASURE_REPRESENTATION_ITEM('density measure',
POSITIVE_RATIO_MEASURE(7850.),#12798);
#12844=MEASURE_REPRESENTATION_ITEM('density measure',
POSITIVE_RATIO_MEASURE(7850.),#12799);
#12845=MEASURE_REPRESENTATION_ITEM('density measure',
POSITIVE_RATIO_MEASURE(7850.),#12800);
#12846=MEASURE_REPRESENTATION_ITEM('density measure',
POSITIVE_RATIO_MEASURE(7850.),#12801);
#12847=MEASURE_REPRESENTATION_ITEM('density measure',
POSITIVE_RATIO_MEASURE(7850.),#12802);
#12848=MEASURE_REPRESENTATION_ITEM('density measure',
POSITIVE_RATIO_MEASURE(7850.),#12803);
#12849=MEASURE_REPRESENTATION_ITEM('density measure',
POSITIVE_RATIO_MEASURE(7850.),#12804);
#12850=MEASURE_REPRESENTATION_ITEM('density measure',
POSITIVE_RATIO_MEASURE(7850.),#12805);
#12851=MEASURE_REPRESENTATION_ITEM('density measure',
POSITIVE_RATIO_MEASURE(7850.),#12806);
#12852=MEASURE_REPRESENTATION_ITEM('density measure',
POSITIVE_RATIO_MEASURE(7850.),#12807);
#12853=MEASURE_REPRESENTATION_ITEM('density measure',
POSITIVE_RATIO_MEASURE(7850.),#12808);
#12854=MEASURE_REPRESENTATION_ITEM('density measure',
POSITIVE_RATIO_MEASURE(7850.),#12809);
#12855=MEASURE_REPRESENTATION_ITEM('density measure',
POSITIVE_RATIO_MEASURE(7850.),#12810);
#12856=MEASURE_REPRESENTATION_ITEM('density measure',
POSITIVE_RATIO_MEASURE(7850.),#12811);
#12857=MEASURE_REPRESENTATION_ITEM('density measure',
POSITIVE_RATIO_MEASURE(7850.),#12812);
#12858=MEASURE_REPRESENTATION_ITEM('density measure',
POSITIVE_RATIO_MEASURE(7850.),#12813);
#12859=MEASURE_REPRESENTATION_ITEM('density measure',
POSITIVE_RATIO_MEASURE(7850.),#12814);
#12860=MEASURE_REPRESENTATION_ITEM('density measure',
POSITIVE_RATIO_MEASURE(7850.),#12815);
#12861=MEASURE_REPRESENTATION_ITEM('density measure',
POSITIVE_RATIO_MEASURE(7850.),#12816);
#12862=MEASURE_REPRESENTATION_ITEM('density measure',
POSITIVE_RATIO_MEASURE(7850.),#12817);
#12863=MEASURE_REPRESENTATION_ITEM('density measure',
POSITIVE_RATIO_MEASURE(7850.),#12818);
#12864=MEASURE_REPRESENTATION_ITEM('density measure',
POSITIVE_RATIO_MEASURE(7850.),#12819);
#12865=MEASURE_REPRESENTATION_ITEM('density measure',
POSITIVE_RATIO_MEASURE(7850.),#12820);
#12866=MEASURE_REPRESENTATION_ITEM('density measure',
POSITIVE_RATIO_MEASURE(7850.),#12821);
#12867=MEASURE_REPRESENTATION_ITEM('density measure',
POSITIVE_RATIO_MEASURE(7850.),#12822);
#12868=MEASURE_REPRESENTATION_ITEM('density measure',
POSITIVE_RATIO_MEASURE(7850.),#12823);
#12869=MEASURE_REPRESENTATION_ITEM('density measure',
POSITIVE_RATIO_MEASURE(7850.),#12824);
#12870=MEASURE_REPRESENTATION_ITEM('density measure',
POSITIVE_RATIO_MEASURE(7850.),#12825);
#12871=MEASURE_REPRESENTATION_ITEM('density measure',
POSITIVE_RATIO_MEASURE(7850.),#12826);
#12872=MEASURE_REPRESENTATION_ITEM('density measure',
POSITIVE_RATIO_MEASURE(7850.),#12827);
#12873=PROPERTY_DEFINITION_REPRESENTATION(#13098,#12963);
#12874=PROPERTY_DEFINITION_REPRESENTATION(#13099,#12964);
#12875=PROPERTY_DEFINITION_REPRESENTATION(#13100,#12965);
#12876=PROPERTY_DEFINITION_REPRESENTATION(#13101,#12966);
#12877=PROPERTY_DEFINITION_REPRESENTATION(#13102,#12967);
#12878=PROPERTY_DEFINITION_REPRESENTATION(#13103,#12968);
#12879=PROPERTY_DEFINITION_REPRESENTATION(#13104,#12969);
#12880=PROPERTY_DEFINITION_REPRESENTATION(#13105,#12970);
#12881=PROPERTY_DEFINITION_REPRESENTATION(#13106,#12971);
#12882=PROPERTY_DEFINITION_REPRESENTATION(#13107,#12972);
#12883=PROPERTY_DEFINITION_REPRESENTATION(#13108,#12973);
#12884=PROPERTY_DEFINITION_REPRESENTATION(#13109,#12974);
#12885=PROPERTY_DEFINITION_REPRESENTATION(#13110,#12975);
#12886=PROPERTY_DEFINITION_REPRESENTATION(#13111,#12976);
#12887=PROPERTY_DEFINITION_REPRESENTATION(#13112,#12977);
#12888=PROPERTY_DEFINITION_REPRESENTATION(#13113,#12978);
#12889=PROPERTY_DEFINITION_REPRESENTATION(#13114,#12979);
#12890=PROPERTY_DEFINITION_REPRESENTATION(#13115,#12980);
#12891=PROPERTY_DEFINITION_REPRESENTATION(#13116,#12981);
#12892=PROPERTY_DEFINITION_REPRESENTATION(#13117,#12982);
#12893=PROPERTY_DEFINITION_REPRESENTATION(#13118,#12983);
#12894=PROPERTY_DEFINITION_REPRESENTATION(#13119,#12984);
#12895=PROPERTY_DEFINITION_REPRESENTATION(#13120,#12985);
#12896=PROPERTY_DEFINITION_REPRESENTATION(#13121,#12986);
#12897=PROPERTY_DEFINITION_REPRESENTATION(#13122,#12987);
#12898=PROPERTY_DEFINITION_REPRESENTATION(#13123,#12988);
#12899=PROPERTY_DEFINITION_REPRESENTATION(#13124,#12989);
#12900=PROPERTY_DEFINITION_REPRESENTATION(#13125,#12990);
#12901=PROPERTY_DEFINITION_REPRESENTATION(#13126,#12991);
#12902=PROPERTY_DEFINITION_REPRESENTATION(#13127,#12992);
#12903=PROPERTY_DEFINITION_REPRESENTATION(#13128,#12993);
#12904=PROPERTY_DEFINITION_REPRESENTATION(#13129,#12994);
#12905=PROPERTY_DEFINITION_REPRESENTATION(#13130,#12995);
#12906=PROPERTY_DEFINITION_REPRESENTATION(#13131,#12996);
#12907=PROPERTY_DEFINITION_REPRESENTATION(#13132,#12997);
#12908=PROPERTY_DEFINITION_REPRESENTATION(#13133,#12998);
#12909=PROPERTY_DEFINITION_REPRESENTATION(#13134,#12999);
#12910=PROPERTY_DEFINITION_REPRESENTATION(#13135,#13000);
#12911=PROPERTY_DEFINITION_REPRESENTATION(#13136,#13001);
#12912=PROPERTY_DEFINITION_REPRESENTATION(#13137,#13002);
#12913=PROPERTY_DEFINITION_REPRESENTATION(#13138,#13003);
#12914=PROPERTY_DEFINITION_REPRESENTATION(#13139,#13004);
#12915=PROPERTY_DEFINITION_REPRESENTATION(#13140,#13005);
#12916=PROPERTY_DEFINITION_REPRESENTATION(#13141,#13006);
#12917=PROPERTY_DEFINITION_REPRESENTATION(#13142,#13007);
#12918=PROPERTY_DEFINITION_REPRESENTATION(#13143,#13008);
#12919=PROPERTY_DEFINITION_REPRESENTATION(#13144,#13009);
#12920=PROPERTY_DEFINITION_REPRESENTATION(#13145,#13010);
#12921=PROPERTY_DEFINITION_REPRESENTATION(#13146,#13011);
#12922=PROPERTY_DEFINITION_REPRESENTATION(#13147,#13012);
#12923=PROPERTY_DEFINITION_REPRESENTATION(#13148,#13013);
#12924=PROPERTY_DEFINITION_REPRESENTATION(#13149,#13014);
#12925=PROPERTY_DEFINITION_REPRESENTATION(#13150,#13015);
#12926=PROPERTY_DEFINITION_REPRESENTATION(#13151,#13016);
#12927=PROPERTY_DEFINITION_REPRESENTATION(#13152,#13017);
#12928=PROPERTY_DEFINITION_REPRESENTATION(#13153,#13018);
#12929=PROPERTY_DEFINITION_REPRESENTATION(#13154,#13019);
#12930=PROPERTY_DEFINITION_REPRESENTATION(#13155,#13020);
#12931=PROPERTY_DEFINITION_REPRESENTATION(#13156,#13021);
#12932=PROPERTY_DEFINITION_REPRESENTATION(#13157,#13022);
#12933=PROPERTY_DEFINITION_REPRESENTATION(#13158,#13023);
#12934=PROPERTY_DEFINITION_REPRESENTATION(#13159,#13024);
#12935=PROPERTY_DEFINITION_REPRESENTATION(#13160,#13025);
#12936=PROPERTY_DEFINITION_REPRESENTATION(#13161,#13026);
#12937=PROPERTY_DEFINITION_REPRESENTATION(#13162,#13027);
#12938=PROPERTY_DEFINITION_REPRESENTATION(#13163,#13028);
#12939=PROPERTY_DEFINITION_REPRESENTATION(#13164,#13029);
#12940=PROPERTY_DEFINITION_REPRESENTATION(#13165,#13030);
#12941=PROPERTY_DEFINITION_REPRESENTATION(#13166,#13031);
#12942=PROPERTY_DEFINITION_REPRESENTATION(#13167,#13032);
#12943=PROPERTY_DEFINITION_REPRESENTATION(#13168,#13033);
#12944=PROPERTY_DEFINITION_REPRESENTATION(#13169,#13034);
#12945=PROPERTY_DEFINITION_REPRESENTATION(#13170,#13035);
#12946=PROPERTY_DEFINITION_REPRESENTATION(#13171,#13036);
#12947=PROPERTY_DEFINITION_REPRESENTATION(#13172,#13037);
#12948=PROPERTY_DEFINITION_REPRESENTATION(#13173,#13038);
#12949=PROPERTY_DEFINITION_REPRESENTATION(#13174,#13039);
#12950=PROPERTY_DEFINITION_REPRESENTATION(#13175,#13040);
#12951=PROPERTY_DEFINITION_REPRESENTATION(#13176,#13041);
#12952=PROPERTY_DEFINITION_REPRESENTATION(#13177,#13042);
#12953=PROPERTY_DEFINITION_REPRESENTATION(#13178,#13043);
#12954=PROPERTY_DEFINITION_REPRESENTATION(#13179,#13044);
#12955=PROPERTY_DEFINITION_REPRESENTATION(#13180,#13045);
#12956=PROPERTY_DEFINITION_REPRESENTATION(#13181,#13046);
#12957=PROPERTY_DEFINITION_REPRESENTATION(#13182,#13047);
#12958=PROPERTY_DEFINITION_REPRESENTATION(#13183,#13048);
#12959=PROPERTY_DEFINITION_REPRESENTATION(#13184,#13049);
#12960=PROPERTY_DEFINITION_REPRESENTATION(#13185,#13050);
#12961=PROPERTY_DEFINITION_REPRESENTATION(#13186,#13051);
#12962=PROPERTY_DEFINITION_REPRESENTATION(#13187,#13052);
#12963=REPRESENTATION('material name',(#13053),#33250);
#12964=REPRESENTATION('density',(#12828),#33250);
#12965=REPRESENTATION('material name',(#13054),#33251);
#12966=REPRESENTATION('density',(#12829),#33251);
#12967=REPRESENTATION('material name',(#13055),#33252);
#12968=REPRESENTATION('density',(#12830),#33252);
#12969=REPRESENTATION('material name',(#13056),#33253);
#12970=REPRESENTATION('density',(#12831),#33253);
#12971=REPRESENTATION('material name',(#13057),#33254);
#12972=REPRESENTATION('density',(#12832),#33254);
#12973=REPRESENTATION('material name',(#13058),#33255);
#12974=REPRESENTATION('density',(#12833),#33255);
#12975=REPRESENTATION('material name',(#13059),#33256);
#12976=REPRESENTATION('density',(#12834),#33256);
#12977=REPRESENTATION('material name',(#13060),#33257);
#12978=REPRESENTATION('density',(#12835),#33257);
#12979=REPRESENTATION('material name',(#13061),#33258);
#12980=REPRESENTATION('density',(#12836),#33258);
#12981=REPRESENTATION('material name',(#13062),#33259);
#12982=REPRESENTATION('density',(#12837),#33259);
#12983=REPRESENTATION('material name',(#13063),#33260);
#12984=REPRESENTATION('density',(#12838),#33260);
#12985=REPRESENTATION('material name',(#13064),#33261);
#12986=REPRESENTATION('density',(#12839),#33261);
#12987=REPRESENTATION('material name',(#13065),#33262);
#12988=REPRESENTATION('density',(#12840),#33262);
#12989=REPRESENTATION('material name',(#13066),#33263);
#12990=REPRESENTATION('density',(#12841),#33263);
#12991=REPRESENTATION('material name',(#13067),#33264);
#12992=REPRESENTATION('density',(#12842),#33264);
#12993=REPRESENTATION('material name',(#13068),#33265);
#12994=REPRESENTATION('density',(#12843),#33265);
#12995=REPRESENTATION('material name',(#13069),#33266);
#12996=REPRESENTATION('density',(#12844),#33266);
#12997=REPRESENTATION('material name',(#13070),#33268);
#12998=REPRESENTATION('density',(#12845),#33268);
#12999=REPRESENTATION('material name',(#13071),#33269);
#13000=REPRESENTATION('density',(#12846),#33269);
#13001=REPRESENTATION('material name',(#13072),#33270);
#13002=REPRESENTATION('density',(#12847),#33270);
#13003=REPRESENTATION('material name',(#13073),#33271);
#13004=REPRESENTATION('density',(#12848),#33271);
#13005=REPRESENTATION('material name',(#13074),#33272);
#13006=REPRESENTATION('density',(#12849),#33272);
#13007=REPRESENTATION('material name',(#13075),#33273);
#13008=REPRESENTATION('density',(#12850),#33273);
#13009=REPRESENTATION('material name',(#13076),#33275);
#13010=REPRESENTATION('density',(#12851),#33275);
#13011=REPRESENTATION('material name',(#13077),#33276);
#13012=REPRESENTATION('density',(#12852),#33276);
#13013=REPRESENTATION('material name',(#13078),#33277);
#13014=REPRESENTATION('density',(#12853),#33277);
#13015=REPRESENTATION('material name',(#13079),#33278);
#13016=REPRESENTATION('density',(#12854),#33278);
#13017=REPRESENTATION('material name',(#13080),#33279);
#13018=REPRESENTATION('density',(#12855),#33279);
#13019=REPRESENTATION('material name',(#13081),#33280);
#13020=REPRESENTATION('density',(#12856),#33280);
#13021=REPRESENTATION('material name',(#13082),#33282);
#13022=REPRESENTATION('density',(#12857),#33282);
#13023=REPRESENTATION('material name',(#13083),#33283);
#13024=REPRESENTATION('density',(#12858),#33283);
#13025=REPRESENTATION('material name',(#13084),#33284);
#13026=REPRESENTATION('density',(#12859),#33284);
#13027=REPRESENTATION('material name',(#13085),#33285);
#13028=REPRESENTATION('density',(#12860),#33285);
#13029=REPRESENTATION('material name',(#13086),#33286);
#13030=REPRESENTATION('density',(#12861),#33286);
#13031=REPRESENTATION('material name',(#13087),#33287);
#13032=REPRESENTATION('density',(#12862),#33287);
#13033=REPRESENTATION('material name',(#13088),#33288);
#13034=REPRESENTATION('density',(#12863),#33288);
#13035=REPRESENTATION('material name',(#13089),#33289);
#13036=REPRESENTATION('density',(#12864),#33289);
#13037=REPRESENTATION('material name',(#13090),#33290);
#13038=REPRESENTATION('density',(#12865),#33290);
#13039=REPRESENTATION('material name',(#13091),#33291);
#13040=REPRESENTATION('density',(#12866),#33291);
#13041=REPRESENTATION('material name',(#13092),#33292);
#13042=REPRESENTATION('density',(#12867),#33292);
#13043=REPRESENTATION('material name',(#13093),#33293);
#13044=REPRESENTATION('density',(#12868),#33293);
#13045=REPRESENTATION('material name',(#13094),#33294);
#13046=REPRESENTATION('density',(#12869),#33294);
#13047=REPRESENTATION('material name',(#13095),#33295);
#13048=REPRESENTATION('density',(#12870),#33295);
#13049=REPRESENTATION('material name',(#13096),#33296);
#13050=REPRESENTATION('density',(#12871),#33296);
#13051=REPRESENTATION('material name',(#13097),#33298);
#13052=REPRESENTATION('density',(#12872),#33298);
#13053=DESCRIPTIVE_REPRESENTATION_ITEM('Steel','Steel');
#13054=DESCRIPTIVE_REPRESENTATION_ITEM('Steel','Steel');
#13055=DESCRIPTIVE_REPRESENTATION_ITEM('Steel','Steel');
#13056=DESCRIPTIVE_REPRESENTATION_ITEM('Steel','Steel');
#13057=DESCRIPTIVE_REPRESENTATION_ITEM('Steel','Steel');
#13058=DESCRIPTIVE_REPRESENTATION_ITEM('Steel','Steel');
#13059=DESCRIPTIVE_REPRESENTATION_ITEM('Steel','Steel');
#13060=DESCRIPTIVE_REPRESENTATION_ITEM('Steel','Steel');
#13061=DESCRIPTIVE_REPRESENTATION_ITEM('Steel','Steel');
#13062=DESCRIPTIVE_REPRESENTATION_ITEM('Steel','Steel');
#13063=DESCRIPTIVE_REPRESENTATION_ITEM('Steel','Steel');
#13064=DESCRIPTIVE_REPRESENTATION_ITEM('Steel','Steel');
#13065=DESCRIPTIVE_REPRESENTATION_ITEM('Steel','Steel');
#13066=DESCRIPTIVE_REPRESENTATION_ITEM('Steel','Steel');
#13067=DESCRIPTIVE_REPRESENTATION_ITEM('Steel','Steel');
#13068=DESCRIPTIVE_REPRESENTATION_ITEM('Steel','Steel');
#13069=DESCRIPTIVE_REPRESENTATION_ITEM('Steel','Steel');
#13070=DESCRIPTIVE_REPRESENTATION_ITEM('Steel','Steel');
#13071=DESCRIPTIVE_REPRESENTATION_ITEM('Steel','Steel');
#13072=DESCRIPTIVE_REPRESENTATION_ITEM('Steel','Steel');
#13073=DESCRIPTIVE_REPRESENTATION_ITEM('Steel','Steel');
#13074=DESCRIPTIVE_REPRESENTATION_ITEM('Steel','Steel');
#13075=DESCRIPTIVE_REPRESENTATION_ITEM('Steel','Steel');
#13076=DESCRIPTIVE_REPRESENTATION_ITEM('Steel','Steel');
#13077=DESCRIPTIVE_REPRESENTATION_ITEM('Steel','Steel');
#13078=DESCRIPTIVE_REPRESENTATION_ITEM('Steel','Steel');
#13079=DESCRIPTIVE_REPRESENTATION_ITEM('Steel','Steel');
#13080=DESCRIPTIVE_REPRESENTATION_ITEM('Steel','Steel');
#13081=DESCRIPTIVE_REPRESENTATION_ITEM('Steel','Steel');
#13082=DESCRIPTIVE_REPRESENTATION_ITEM('Steel','Steel');
#13083=DESCRIPTIVE_REPRESENTATION_ITEM('Steel','Steel');
#13084=DESCRIPTIVE_REPRESENTATION_ITEM('Steel','Steel');
#13085=DESCRIPTIVE_REPRESENTATION_ITEM('Steel','Steel');
#13086=DESCRIPTIVE_REPRESENTATION_ITEM('Steel','Steel');
#13087=DESCRIPTIVE_REPRESENTATION_ITEM('Steel','Steel');
#13088=DESCRIPTIVE_REPRESENTATION_ITEM('Steel','Steel');
#13089=DESCRIPTIVE_REPRESENTATION_ITEM('Steel','Steel');
#13090=DESCRIPTIVE_REPRESENTATION_ITEM('Steel','Steel');
#13091=DESCRIPTIVE_REPRESENTATION_ITEM('Steel','Steel');
#13092=DESCRIPTIVE_REPRESENTATION_ITEM('Steel','Steel');
#13093=DESCRIPTIVE_REPRESENTATION_ITEM('Steel','Steel');
#13094=DESCRIPTIVE_REPRESENTATION_ITEM('Steel','Steel');
#13095=DESCRIPTIVE_REPRESENTATION_ITEM('Steel','Steel');
#13096=DESCRIPTIVE_REPRESENTATION_ITEM('Steel','Steel');
#13097=DESCRIPTIVE_REPRESENTATION_ITEM('Steel','Steel');
#13098=PROPERTY_DEFINITION('material property','material name',#33540);
#13099=PROPERTY_DEFINITION('material property','density of part',#33540);
#13100=PROPERTY_DEFINITION('material property','material name',#33541);
#13101=PROPERTY_DEFINITION('material property','density of part',#33541);
#13102=PROPERTY_DEFINITION('material property','material name',#33542);
#13103=PROPERTY_DEFINITION('material property','density of part',#33542);
#13104=PROPERTY_DEFINITION('material property','material name',#33543);
#13105=PROPERTY_DEFINITION('material property','density of part',#33543);
#13106=PROPERTY_DEFINITION('material property','material name',#33544);
#13107=PROPERTY_DEFINITION('material property','density of part',#33544);
#13108=PROPERTY_DEFINITION('material property','material name',#33545);
#13109=PROPERTY_DEFINITION('material property','density of part',#33545);
#13110=PROPERTY_DEFINITION('material property','material name',#33546);
#13111=PROPERTY_DEFINITION('material property','density of part',#33546);
#13112=PROPERTY_DEFINITION('material property','material name',#33547);
#13113=PROPERTY_DEFINITION('material property','density of part',#33547);
#13114=PROPERTY_DEFINITION('material property','material name',#33548);
#13115=PROPERTY_DEFINITION('material property','density of part',#33548);
#13116=PROPERTY_DEFINITION('material property','material name',#33549);
#13117=PROPERTY_DEFINITION('material property','density of part',#33549);
#13118=PROPERTY_DEFINITION('material property','material name',#33550);
#13119=PROPERTY_DEFINITION('material property','density of part',#33550);
#13120=PROPERTY_DEFINITION('material property','material name',#33551);
#13121=PROPERTY_DEFINITION('material property','density of part',#33551);
#13122=PROPERTY_DEFINITION('material property','material name',#33552);
#13123=PROPERTY_DEFINITION('material property','density of part',#33552);
#13124=PROPERTY_DEFINITION('material property','material name',#33553);
#13125=PROPERTY_DEFINITION('material property','density of part',#33553);
#13126=PROPERTY_DEFINITION('material property','material name',#33554);
#13127=PROPERTY_DEFINITION('material property','density of part',#33554);
#13128=PROPERTY_DEFINITION('material property','material name',#33555);
#13129=PROPERTY_DEFINITION('material property','density of part',#33555);
#13130=PROPERTY_DEFINITION('material property','material name',#33556);
#13131=PROPERTY_DEFINITION('material property','density of part',#33556);
#13132=PROPERTY_DEFINITION('material property','material name',#33558);
#13133=PROPERTY_DEFINITION('material property','density of part',#33558);
#13134=PROPERTY_DEFINITION('material property','material name',#33559);
#13135=PROPERTY_DEFINITION('material property','density of part',#33559);
#13136=PROPERTY_DEFINITION('material property','material name',#33560);
#13137=PROPERTY_DEFINITION('material property','density of part',#33560);
#13138=PROPERTY_DEFINITION('material property','material name',#33561);
#13139=PROPERTY_DEFINITION('material property','density of part',#33561);
#13140=PROPERTY_DEFINITION('material property','material name',#33562);
#13141=PROPERTY_DEFINITION('material property','density of part',#33562);
#13142=PROPERTY_DEFINITION('material property','material name',#33563);
#13143=PROPERTY_DEFINITION('material property','density of part',#33563);
#13144=PROPERTY_DEFINITION('material property','material name',#33565);
#13145=PROPERTY_DEFINITION('material property','density of part',#33565);
#13146=PROPERTY_DEFINITION('material property','material name',#33566);
#13147=PROPERTY_DEFINITION('material property','density of part',#33566);
#13148=PROPERTY_DEFINITION('material property','material name',#33567);
#13149=PROPERTY_DEFINITION('material property','density of part',#33567);
#13150=PROPERTY_DEFINITION('material property','material name',#33568);
#13151=PROPERTY_DEFINITION('material property','density of part',#33568);
#13152=PROPERTY_DEFINITION('material property','material name',#33569);
#13153=PROPERTY_DEFINITION('material property','density of part',#33569);
#13154=PROPERTY_DEFINITION('material property','material name',#33570);
#13155=PROPERTY_DEFINITION('material property','density of part',#33570);
#13156=PROPERTY_DEFINITION('material property','material name',#33572);
#13157=PROPERTY_DEFINITION('material property','density of part',#33572);
#13158=PROPERTY_DEFINITION('material property','material name',#33573);
#13159=PROPERTY_DEFINITION('material property','density of part',#33573);
#13160=PROPERTY_DEFINITION('material property','material name',#33574);
#13161=PROPERTY_DEFINITION('material property','density of part',#33574);
#13162=PROPERTY_DEFINITION('material property','material name',#33575);
#13163=PROPERTY_DEFINITION('material property','density of part',#33575);
#13164=PROPERTY_DEFINITION('material property','material name',#33576);
#13165=PROPERTY_DEFINITION('material property','density of part',#33576);
#13166=PROPERTY_DEFINITION('material property','material name',#33577);
#13167=PROPERTY_DEFINITION('material property','density of part',#33577);
#13168=PROPERTY_DEFINITION('material property','material name',#33578);
#13169=PROPERTY_DEFINITION('material property','density of part',#33578);
#13170=PROPERTY_DEFINITION('material property','material name',#33579);
#13171=PROPERTY_DEFINITION('material property','density of part',#33579);
#13172=PROPERTY_DEFINITION('material property','material name',#33580);
#13173=PROPERTY_DEFINITION('material property','density of part',#33580);
#13174=PROPERTY_DEFINITION('material property','material name',#33581);
#13175=PROPERTY_DEFINITION('material property','density of part',#33581);
#13176=PROPERTY_DEFINITION('material property','material name',#33582);
#13177=PROPERTY_DEFINITION('material property','density of part',#33582);
#13178=PROPERTY_DEFINITION('material property','material name',#33583);
#13179=PROPERTY_DEFINITION('material property','density of part',#33583);
#13180=PROPERTY_DEFINITION('material property','material name',#33584);
#13181=PROPERTY_DEFINITION('material property','density of part',#33584);
#13182=PROPERTY_DEFINITION('material property','material name',#33585);
#13183=PROPERTY_DEFINITION('material property','density of part',#33585);
#13184=PROPERTY_DEFINITION('material property','material name',#33586);
#13185=PROPERTY_DEFINITION('material property','density of part',#33586);
#13186=PROPERTY_DEFINITION('material property','material name',#33588);
#13187=PROPERTY_DEFINITION('material property','density of part',#33588);
#13188=AXIS2_PLACEMENT_3D('',#17890,#14367,#14368);
#13189=AXIS2_PLACEMENT_3D('',#17891,#14369,#14370);
#13190=AXIS2_PLACEMENT_3D('',#17892,#14371,#14372);
#13191=AXIS2_PLACEMENT_3D('',#17893,#14373,#14374);
#13192=AXIS2_PLACEMENT_3D('',#17895,#14375,#14376);
#13193=AXIS2_PLACEMENT_3D('',#17898,#14378,#14379);
#13194=AXIS2_PLACEMENT_3D('',#17899,#14380,#14381);
#13195=AXIS2_PLACEMENT_3D('',#17901,#14382,#14383);
#13196=AXIS2_PLACEMENT_3D('',#17904,#14385,#14386);
#13197=AXIS2_PLACEMENT_3D('',#17905,#14387,#14388);
#13198=AXIS2_PLACEMENT_3D('',#17907,#14389,#14390);
#13199=AXIS2_PLACEMENT_3D('',#17910,#14392,#14393);
#13200=AXIS2_PLACEMENT_3D('',#17911,#14394,#14395);
#13201=AXIS2_PLACEMENT_3D('',#17913,#14396,#14397);
#13202=AXIS2_PLACEMENT_3D('',#17916,#14399,#14400);
#13203=AXIS2_PLACEMENT_3D('',#17917,#14401,#14402);
#13204=AXIS2_PLACEMENT_3D('',#17919,#14403,#14404);
#13205=AXIS2_PLACEMENT_3D('',#17922,#14406,#14407);
#13206=AXIS2_PLACEMENT_3D('',#17923,#14408,#14409);
#13207=AXIS2_PLACEMENT_3D('',#17925,#14410,#14411);
#13208=AXIS2_PLACEMENT_3D('',#17928,#14413,#14414);
#13209=AXIS2_PLACEMENT_3D('',#17929,#14415,#14416);
#13210=AXIS2_PLACEMENT_3D('',#17938,#14421,#14422);
#13211=AXIS2_PLACEMENT_3D('',#17944,#14426,#14427);
#13212=AXIS2_PLACEMENT_3D('',#17950,#14431,#14432);
#13213=AXIS2_PLACEMENT_3D('',#17953,#14435,#14436);
#13214=AXIS2_PLACEMENT_3D('',#17954,#14437,#14438);
#13215=AXIS2_PLACEMENT_3D('',#17955,#14439,#14440);
#13216=AXIS2_PLACEMENT_3D('',#17956,#14441,#14442);
#13217=AXIS2_PLACEMENT_3D('',#17965,#14447,#14448);
#13218=AXIS2_PLACEMENT_3D('',#17971,#14452,#14453);
#13219=AXIS2_PLACEMENT_3D('',#17977,#14457,#14458);
#13220=AXIS2_PLACEMENT_3D('',#17980,#14461,#14462);
#13221=AXIS2_PLACEMENT_3D('',#17981,#14463,#14464);
#13222=AXIS2_PLACEMENT_3D('',#17982,#14465,#14466);
#13223=AXIS2_PLACEMENT_3D('',#17983,#14467,#14468);
#13224=AXIS2_PLACEMENT_3D('',#17992,#14473,#14474);
#13225=AXIS2_PLACEMENT_3D('',#17998,#14478,#14479);
#13226=AXIS2_PLACEMENT_3D('',#18004,#14483,#14484);
#13227=AXIS2_PLACEMENT_3D('',#18007,#14487,#14488);
#13228=AXIS2_PLACEMENT_3D('',#18008,#14489,#14490);
#13229=AXIS2_PLACEMENT_3D('',#18009,#14491,#14492);
#13230=AXIS2_PLACEMENT_3D('',#18010,#14493,#14494);
#13231=AXIS2_PLACEMENT_3D('',#18012,#14495,#14496);
#13232=AXIS2_PLACEMENT_3D('',#18015,#14498,#14499);
#13233=AXIS2_PLACEMENT_3D('',#18016,#14500,#14501);
#13234=AXIS2_PLACEMENT_3D('',#18017,#14502,#14503);
#13235=AXIS2_PLACEMENT_3D('',#18019,#14504,#14505);
#13236=AXIS2_PLACEMENT_3D('',#18022,#14507,#14508);
#13237=AXIS2_PLACEMENT_3D('',#18023,#14509,#14510);
#13238=AXIS2_PLACEMENT_3D('',#18024,#14511,#14512);
#13239=AXIS2_PLACEMENT_3D('',#18033,#14517,#14518);
#13240=AXIS2_PLACEMENT_3D('',#18042,#14523,#14524);
#13241=AXIS2_PLACEMENT_3D('',#18044,#14525,#14526);
#13242=AXIS2_PLACEMENT_3D('',#18051,#14530,#14531);
#13243=AXIS2_PLACEMENT_3D('',#18052,#14532,#14533);
#13244=AXIS2_PLACEMENT_3D('',#18053,#14534,#14535);
#13245=AXIS2_PLACEMENT_3D('',#18054,#14536,#14537);
#13246=AXIS2_PLACEMENT_3D('',#18055,#14538,#14539);
#13247=AXIS2_PLACEMENT_3D('',#18058,#14541,#14542);
#13248=AXIS2_PLACEMENT_3D('',#18059,#14543,#14544);
#13249=AXIS2_PLACEMENT_3D('',#18061,#14545,#14546);
#13250=AXIS2_PLACEMENT_3D('',#18063,#14548,#14549);
#13251=AXIS2_PLACEMENT_3D('',#18069,#14553,#14554);
#13252=AXIS2_PLACEMENT_3D('',#18071,#14556,#14557);
#13253=AXIS2_PLACEMENT_3D('',#18073,#14559,#14560);
#13254=AXIS2_PLACEMENT_3D('',#18075,#14561,#14562);
#13255=AXIS2_PLACEMENT_3D('',#18078,#14564,#14565);
#13256=AXIS2_PLACEMENT_3D('',#18079,#14566,#14567);
#13257=AXIS2_PLACEMENT_3D('',#18080,#14568,#14569);
#13258=AXIS2_PLACEMENT_3D('',#18082,#14570,#14571);
#13259=AXIS2_PLACEMENT_3D('',#18085,#14573,#14574);
#13260=AXIS2_PLACEMENT_3D('',#18086,#14575,#14576);
#13261=AXIS2_PLACEMENT_3D('',#18087,#14577,#14578);
#13262=AXIS2_PLACEMENT_3D('',#18096,#14583,#14584);
#13263=AXIS2_PLACEMENT_3D('',#18105,#14589,#14590);
#13264=AXIS2_PLACEMENT_3D('',#18107,#14591,#14592);
#13265=AXIS2_PLACEMENT_3D('',#18117,#14597,#14598);
#13266=AXIS2_PLACEMENT_3D('',#18119,#14599,#14600);
#13267=AXIS2_PLACEMENT_3D('',#18128,#14605,#14606);
#13268=AXIS2_PLACEMENT_3D('',#18129,#14607,#14608);
#13269=AXIS2_PLACEMENT_3D('',#18130,#14609,#14610);
#13270=AXIS2_PLACEMENT_3D('',#18131,#14611,#14612);
#13271=AXIS2_PLACEMENT_3D('',#18132,#14613,#14614);
#13272=AXIS2_PLACEMENT_3D('',#18135,#14616,#14617);
#13273=AXIS2_PLACEMENT_3D('',#18136,#14618,#14619);
#13274=AXIS2_PLACEMENT_3D('',#18138,#14620,#14621);
#13275=AXIS2_PLACEMENT_3D('',#18140,#14623,#14624);
#13276=AXIS2_PLACEMENT_3D('',#18146,#14628,#14629);
#13277=AXIS2_PLACEMENT_3D('',#18148,#14631,#14632);
#13278=AXIS2_PLACEMENT_3D('',#18150,#14634,#14635);
#13279=AXIS2_PLACEMENT_3D('',#18156,#14639,#14640);
#13280=AXIS2_PLACEMENT_3D('',#18160,#14642,#14643);
#13281=AXIS2_PLACEMENT_3D('',#18161,#14644,#14645);
#13282=AXIS2_PLACEMENT_3D('',#18178,#14646,#14647);
#13283=AXIS2_PLACEMENT_3D('',#18235,#14649,#14650);
#13284=AXIS2_PLACEMENT_3D('',#18237,#14652,#14653);
#13285=AXIS2_PLACEMENT_3D('',#18239,#14655,#14656);
#13286=AXIS2_PLACEMENT_3D('',#18240,#14657,#14658);
#13287=AXIS2_PLACEMENT_3D('',#18242,#14659,#14660);
#13288=AXIS2_PLACEMENT_3D('',#18245,#14662,#14663);
#13289=AXIS2_PLACEMENT_3D('',#18246,#14664,#14665);
#13290=AXIS2_PLACEMENT_3D('',#18249,#14667,#14668);
#13291=AXIS2_PLACEMENT_3D('',#18250,#14669,#14670);
#13292=AXIS2_PLACEMENT_3D('',#18251,#14671,#14672);
#13293=AXIS2_PLACEMENT_3D('',#18255,#14675,#14676);
#13294=AXIS2_PLACEMENT_3D('',#18259,#14679,#14680);
#13295=AXIS2_PLACEMENT_3D('',#18261,#14682,#14683);
#13296=AXIS2_PLACEMENT_3D('',#18262,#14684,#14685);
#13297=AXIS2_PLACEMENT_3D('',#18263,#14686,#14687);
#13298=AXIS2_PLACEMENT_3D('',#18264,#14688,#14689);
#13299=AXIS2_PLACEMENT_3D('',#18269,#14691,#14692);
#13300=AXIS2_PLACEMENT_3D('',#18272,#14694,#14695);
#13301=AXIS2_PLACEMENT_3D('',#18273,#14696,#14697);
#13302=AXIS2_PLACEMENT_3D('',#18274,#14698,#14699);
#13303=AXIS2_PLACEMENT_3D('',#18275,#14700,#14701);
#13304=AXIS2_PLACEMENT_3D('',#18280,#14703,#14704);
#13305=AXIS2_PLACEMENT_3D('',#18283,#14706,#14707);
#13306=AXIS2_PLACEMENT_3D('',#18284,#14708,#14709);
#13307=AXIS2_PLACEMENT_3D('',#18285,#14710,#14711);
#13308=AXIS2_PLACEMENT_3D('',#18286,#14712,#14713);
#13309=AXIS2_PLACEMENT_3D('',#18288,#14714,#14715);
#13310=AXIS2_PLACEMENT_3D('',#18290,#14716,#14717);
#13311=AXIS2_PLACEMENT_3D('',#18291,#14718,#14719);
#13312=AXIS2_PLACEMENT_3D('',#18292,#14720,#14721);
#13313=AXIS2_PLACEMENT_3D('',#18294,#14722,#14723);
#13314=AXIS2_PLACEMENT_3D('',#18296,#14724,#14725);
#13315=AXIS2_PLACEMENT_3D('',#18297,#14726,#14727);
#13316=AXIS2_PLACEMENT_3D('',#18301,#14729,#14730);
#13317=AXIS2_PLACEMENT_3D('',#18302,#14731,#14732);
#13318=AXIS2_PLACEMENT_3D('',#18319,#14733,#14734);
#13319=AXIS2_PLACEMENT_3D('',#18376,#14736,#14737);
#13320=AXIS2_PLACEMENT_3D('',#18378,#14739,#14740);
#13321=AXIS2_PLACEMENT_3D('',#18380,#14741,#14742);
#13322=AXIS2_PLACEMENT_3D('',#18382,#14744,#14745);
#13323=AXIS2_PLACEMENT_3D('',#18384,#14746,#14747);
#13324=AXIS2_PLACEMENT_3D('',#18386,#14749,#14750);
#13325=AXIS2_PLACEMENT_3D('',#18388,#14751,#14752);
#13326=AXIS2_PLACEMENT_3D('',#18390,#14754,#14755);
#13327=AXIS2_PLACEMENT_3D('',#18392,#14756,#14757);
#13328=AXIS2_PLACEMENT_3D('',#18393,#14758,#14759);
#13329=AXIS2_PLACEMENT_3D('',#18396,#14761,#14762);
#13330=AXIS2_PLACEMENT_3D('',#18397,#14763,#14764);
#13331=AXIS2_PLACEMENT_3D('',#18400,#14766,#14767);
#13332=AXIS2_PLACEMENT_3D('',#18401,#14768,#14769);
#13333=AXIS2_PLACEMENT_3D('',#18402,#14770,#14771);
#13334=AXIS2_PLACEMENT_3D('',#18403,#14772,#14773);
#13335=AXIS2_PLACEMENT_3D('',#18412,#14778,#14779);
#13336=AXIS2_PLACEMENT_3D('',#18421,#14784,#14785);
#13337=AXIS2_PLACEMENT_3D('',#18431,#14791,#14792);
#13338=AXIS2_PLACEMENT_3D('',#18441,#14798,#14799);
#13339=AXIS2_PLACEMENT_3D('',#18442,#14800,#14801);
#13340=AXIS2_PLACEMENT_3D('',#18443,#14802,#14803);
#13341=AXIS2_PLACEMENT_3D('',#18444,#14804,#14805);
#13342=AXIS2_PLACEMENT_3D('',#18445,#14806,#14807);
#13343=AXIS2_PLACEMENT_3D('',#18446,#14808,#14809);
#13344=AXIS2_PLACEMENT_3D('',#18447,#14810,#14811);
#13345=AXIS2_PLACEMENT_3D('',#18448,#14812,#14813);
#13346=AXIS2_PLACEMENT_3D('',#18449,#14814,#14815);
#13347=AXIS2_PLACEMENT_3D('',#18450,#14816,#14817);
#13348=AXIS2_PLACEMENT_3D('',#18451,#14818,#14819);
#13349=AXIS2_PLACEMENT_3D('',#18452,#14820,#14821);
#13350=AXIS2_PLACEMENT_3D('',#18453,#14822,#14823);
#13351=AXIS2_PLACEMENT_3D('',#18454,#14824,#14825);
#13352=AXIS2_PLACEMENT_3D('',#18456,#14826,#14827);
#13353=AXIS2_PLACEMENT_3D('',#18459,#14829,#14830);
#13354=AXIS2_PLACEMENT_3D('',#18460,#14831,#14832);
#13355=AXIS2_PLACEMENT_3D('',#18462,#14833,#14834);
#13356=AXIS2_PLACEMENT_3D('',#18465,#14836,#14837);
#13357=AXIS2_PLACEMENT_3D('',#18466,#14838,#14839);
#13358=AXIS2_PLACEMENT_3D('',#18475,#14844,#14845);
#13359=AXIS2_PLACEMENT_3D('',#18484,#14850,#14851);
#13360=AXIS2_PLACEMENT_3D('',#18490,#14855,#14856);
#13361=AXIS2_PLACEMENT_3D('',#18496,#14860,#14861);
#13362=AXIS2_PLACEMENT_3D('',#18502,#14865,#14866);
#13363=AXIS2_PLACEMENT_3D('',#18508,#14870,#14871);
#13364=AXIS2_PLACEMENT_3D('',#18509,#14872,#14873);
#13365=AXIS2_PLACEMENT_3D('',#18515,#14877,#14878);
#13366=AXIS2_PLACEMENT_3D('',#18516,#14879,#14880);
#13367=AXIS2_PLACEMENT_3D('',#18517,#14881,#14882);
#13368=AXIS2_PLACEMENT_3D('',#18521,#14885,#14886);
#13369=AXIS2_PLACEMENT_3D('',#18525,#14889,#14890);
#13370=AXIS2_PLACEMENT_3D('',#18527,#14892,#14893);
#13371=AXIS2_PLACEMENT_3D('',#18528,#14894,#14895);
#13372=AXIS2_PLACEMENT_3D('',#18529,#14896,#14897);
#13373=AXIS2_PLACEMENT_3D('',#18538,#14902,#14903);
#13374=AXIS2_PLACEMENT_3D('',#18547,#14908,#14909);
#13375=AXIS2_PLACEMENT_3D('',#18557,#14915,#14916);
#13376=AXIS2_PLACEMENT_3D('',#18567,#14922,#14923);
#13377=AXIS2_PLACEMENT_3D('',#18568,#14924,#14925);
#13378=AXIS2_PLACEMENT_3D('',#18569,#14926,#14927);
#13379=AXIS2_PLACEMENT_3D('',#18570,#14928,#14929);
#13380=AXIS2_PLACEMENT_3D('',#18571,#14930,#14931);
#13381=AXIS2_PLACEMENT_3D('',#18572,#14932,#14933);
#13382=AXIS2_PLACEMENT_3D('',#18573,#14934,#14935);
#13383=AXIS2_PLACEMENT_3D('',#18574,#14936,#14937);
#13384=AXIS2_PLACEMENT_3D('',#18575,#14938,#14939);
#13385=AXIS2_PLACEMENT_3D('',#18576,#14940,#14941);
#13386=AXIS2_PLACEMENT_3D('',#18577,#14942,#14943);
#13387=AXIS2_PLACEMENT_3D('',#18578,#14944,#14945);
#13388=AXIS2_PLACEMENT_3D('',#18579,#14946,#14947);
#13389=AXIS2_PLACEMENT_3D('',#18580,#14948,#14949);
#13390=AXIS2_PLACEMENT_3D('',#18582,#14950,#14951);
#13391=AXIS2_PLACEMENT_3D('',#18585,#14953,#14954);
#13392=AXIS2_PLACEMENT_3D('',#18586,#14955,#14956);
#13393=AXIS2_PLACEMENT_3D('',#18588,#14957,#14958);
#13394=AXIS2_PLACEMENT_3D('',#18591,#14960,#14961);
#13395=AXIS2_PLACEMENT_3D('',#18592,#14962,#14963);
#13396=AXIS2_PLACEMENT_3D('',#18601,#14968,#14969);
#13397=AXIS2_PLACEMENT_3D('',#18610,#14974,#14975);
#13398=AXIS2_PLACEMENT_3D('',#18616,#14979,#14980);
#13399=AXIS2_PLACEMENT_3D('',#18622,#14984,#14985);
#13400=AXIS2_PLACEMENT_3D('',#18628,#14989,#14990);
#13401=AXIS2_PLACEMENT_3D('',#18634,#14994,#14995);
#13402=AXIS2_PLACEMENT_3D('',#18635,#14996,#14997);
#13403=AXIS2_PLACEMENT_3D('',#18641,#15001,#15002);
#13404=AXIS2_PLACEMENT_3D('',#18642,#15003,#15004);
#13405=AXIS2_PLACEMENT_3D('',#18643,#15005,#15006);
#13406=AXIS2_PLACEMENT_3D('',#18647,#15009,#15010);
#13407=AXIS2_PLACEMENT_3D('',#18651,#15013,#15014);
#13408=AXIS2_PLACEMENT_3D('',#18653,#15016,#15017);
#13409=AXIS2_PLACEMENT_3D('',#18654,#15018,#15019);
#13410=AXIS2_PLACEMENT_3D('',#18655,#15020,#15021);
#13411=AXIS2_PLACEMENT_3D('',#18664,#15026,#15027);
#13412=AXIS2_PLACEMENT_3D('',#18670,#15031,#15032);
#13413=AXIS2_PLACEMENT_3D('',#18675,#15035,#15036);
#13414=AXIS2_PLACEMENT_3D('',#18677,#15037,#15038);
#13415=AXIS2_PLACEMENT_3D('',#18678,#15039,#15040);
#13416=AXIS2_PLACEMENT_3D('',#18682,#15043,#15044);
#13417=AXIS2_PLACEMENT_3D('',#18684,#15046,#15047);
#13418=AXIS2_PLACEMENT_3D('',#18686,#15048,#15049);
#13419=AXIS2_PLACEMENT_3D('',#18688,#15050,#15051);
#13420=AXIS2_PLACEMENT_3D('',#18689,#15052,#15053);
#13421=AXIS2_PLACEMENT_3D('',#18693,#15055,#15056);
#13422=AXIS2_PLACEMENT_3D('',#18694,#15057,#15058);
#13423=AXIS2_PLACEMENT_3D('',#18711,#15059,#15060);
#13424=AXIS2_PLACEMENT_3D('',#18768,#15062,#15063);
#13425=AXIS2_PLACEMENT_3D('',#18770,#15065,#15066);
#13426=AXIS2_PLACEMENT_3D('',#18772,#15068,#15069);
#13427=AXIS2_PLACEMENT_3D('',#18774,#15070,#15071);
#13428=AXIS2_PLACEMENT_3D('',#18776,#15073,#15074);
#13429=AXIS2_PLACEMENT_3D('',#18779,#15076,#15077);
#13430=AXIS2_PLACEMENT_3D('',#18780,#15078,#15079);
#13431=AXIS2_PLACEMENT_3D('',#18781,#15080,#15081);
#13432=AXIS2_PLACEMENT_3D('',#18782,#15082,#15083);
#13433=AXIS2_PLACEMENT_3D('',#18784,#15084,#15085);
#13434=AXIS2_PLACEMENT_3D('',#18787,#15087,#15088);
#13435=AXIS2_PLACEMENT_3D('',#18788,#15089,#15090);
#13436=AXIS2_PLACEMENT_3D('',#18790,#15091,#15092);
#13437=AXIS2_PLACEMENT_3D('',#18793,#15094,#15095);
#13438=AXIS2_PLACEMENT_3D('',#18794,#15096,#15097);
#13439=AXIS2_PLACEMENT_3D('',#18796,#15098,#15099);
#13440=AXIS2_PLACEMENT_3D('',#18799,#15101,#15102);
#13441=AXIS2_PLACEMENT_3D('',#18800,#15103,#15104);
#13442=AXIS2_PLACEMENT_3D('',#18802,#15105,#15106);
#13443=AXIS2_PLACEMENT_3D('',#18805,#15108,#15109);
#13444=AXIS2_PLACEMENT_3D('',#18806,#15110,#15111);
#13445=AXIS2_PLACEMENT_3D('',#18808,#15112,#15113);
#13446=AXIS2_PLACEMENT_3D('',#18811,#15115,#15116);
#13447=AXIS2_PLACEMENT_3D('',#18812,#15117,#15118);
#13448=AXIS2_PLACEMENT_3D('',#18814,#15119,#15120);
#13449=AXIS2_PLACEMENT_3D('',#18817,#15122,#15123);
#13450=AXIS2_PLACEMENT_3D('',#18818,#15124,#15125);
#13451=AXIS2_PLACEMENT_3D('',#18820,#15126,#15127);
#13452=AXIS2_PLACEMENT_3D('',#18823,#15129,#15130);
#13453=AXIS2_PLACEMENT_3D('',#18824,#15131,#15132);
#13454=AXIS2_PLACEMENT_3D('',#18833,#15137,#15138);
#13455=AXIS2_PLACEMENT_3D('',#18842,#15143,#15144);
#13456=AXIS2_PLACEMENT_3D('',#18848,#15148,#15149);
#13457=AXIS2_PLACEMENT_3D('',#18854,#15153,#15154);
#13458=AXIS2_PLACEMENT_3D('',#18861,#15159,#15160);
#13459=AXIS2_PLACEMENT_3D('',#18865,#15163,#15164);
#13460=AXIS2_PLACEMENT_3D('',#18870,#15168,#15169);
#13461=AXIS2_PLACEMENT_3D('',#18872,#15171,#15172);
#13462=AXIS2_PLACEMENT_3D('',#18873,#15173,#15174);
#13463=AXIS2_PLACEMENT_3D('',#18874,#15175,#15176);
#13464=AXIS2_PLACEMENT_3D('',#18875,#15177,#15178);
#13465=AXIS2_PLACEMENT_3D('',#18877,#15179,#15180);
#13466=AXIS2_PLACEMENT_3D('',#18880,#15182,#15183);
#13467=AXIS2_PLACEMENT_3D('',#18881,#15184,#15185);
#13468=AXIS2_PLACEMENT_3D('',#18883,#15186,#15187);
#13469=AXIS2_PLACEMENT_3D('',#18886,#15189,#15190);
#13470=AXIS2_PLACEMENT_3D('',#18887,#15191,#15192);
#13471=AXIS2_PLACEMENT_3D('',#18889,#15193,#15194);
#13472=AXIS2_PLACEMENT_3D('',#18892,#15196,#15197);
#13473=AXIS2_PLACEMENT_3D('',#18893,#15198,#15199);
#13474=AXIS2_PLACEMENT_3D('',#18895,#15200,#15201);
#13475=AXIS2_PLACEMENT_3D('',#18898,#15203,#15204);
#13476=AXIS2_PLACEMENT_3D('',#18899,#15205,#15206);
#13477=AXIS2_PLACEMENT_3D('',#18901,#15207,#15208);
#13478=AXIS2_PLACEMENT_3D('',#18904,#15210,#15211);
#13479=AXIS2_PLACEMENT_3D('',#18905,#15212,#15213);
#13480=AXIS2_PLACEMENT_3D('',#18907,#15214,#15215);
#13481=AXIS2_PLACEMENT_3D('',#18908,#15216,#15217);
#13482=AXIS2_PLACEMENT_3D('',#18911,#15219,#15220);
#13483=AXIS2_PLACEMENT_3D('',#18912,#15221,#15222);
#13484=AXIS2_PLACEMENT_3D('',#18914,#15223,#15224);
#13485=AXIS2_PLACEMENT_3D('',#18917,#15226,#15227);
#13486=AXIS2_PLACEMENT_3D('',#18918,#15228,#15229);
#13487=AXIS2_PLACEMENT_3D('',#18919,#15230,#15231);
#13488=AXIS2_PLACEMENT_3D('',#18920,#15232,#15233);
#13489=AXIS2_PLACEMENT_3D('',#18921,#15234,#15235);
#13490=AXIS2_PLACEMENT_3D('',#18923,#15236,#15237);
#13491=AXIS2_PLACEMENT_3D('',#18926,#15239,#15240);
#13492=AXIS2_PLACEMENT_3D('',#18927,#15241,#15242);
#13493=AXIS2_PLACEMENT_3D('',#18929,#15243,#15244);
#13494=AXIS2_PLACEMENT_3D('',#18932,#15246,#15247);
#13495=AXIS2_PLACEMENT_3D('',#18933,#15248,#15249);
#13496=AXIS2_PLACEMENT_3D('',#18935,#15250,#15251);
#13497=AXIS2_PLACEMENT_3D('',#18938,#15253,#15254);
#13498=AXIS2_PLACEMENT_3D('',#18939,#15255,#15256);
#13499=AXIS2_PLACEMENT_3D('',#18941,#15257,#15258);
#13500=AXIS2_PLACEMENT_3D('',#18944,#15260,#15261);
#13501=AXIS2_PLACEMENT_3D('',#18945,#15262,#15263);
#13502=AXIS2_PLACEMENT_3D('',#18947,#15264,#15265);
#13503=AXIS2_PLACEMENT_3D('',#18950,#15267,#15268);
#13504=AXIS2_PLACEMENT_3D('',#18951,#15269,#15270);
#13505=AXIS2_PLACEMENT_3D('',#18953,#15271,#15272);
#13506=AXIS2_PLACEMENT_3D('',#18954,#15273,#15274);
#13507=AXIS2_PLACEMENT_3D('',#18956,#15275,#15276);
#13508=AXIS2_PLACEMENT_3D('',#18958,#15278,#15279);
#13509=AXIS2_PLACEMENT_3D('',#18960,#15280,#15281);
#13510=AXIS2_PLACEMENT_3D('',#18963,#15283,#15284);
#13511=AXIS2_PLACEMENT_3D('',#18964,#15285,#15286);
#13512=AXIS2_PLACEMENT_3D('',#18965,#15287,#15288);
#13513=AXIS2_PLACEMENT_3D('',#18966,#15289,#15290);
#13514=AXIS2_PLACEMENT_3D('',#18967,#15291,#15292);
#13515=AXIS2_PLACEMENT_3D('',#18969,#15293,#15294);
#13516=AXIS2_PLACEMENT_3D('',#18972,#15296,#15297);
#13517=AXIS2_PLACEMENT_3D('',#18973,#15298,#15299);
#13518=AXIS2_PLACEMENT_3D('',#18975,#15300,#15301);
#13519=AXIS2_PLACEMENT_3D('',#18978,#15303,#15304);
#13520=AXIS2_PLACEMENT_3D('',#18979,#15305,#15306);
#13521=AXIS2_PLACEMENT_3D('',#18981,#15307,#15308);
#13522=AXIS2_PLACEMENT_3D('',#18984,#15310,#15311);
#13523=AXIS2_PLACEMENT_3D('',#18985,#15312,#15313);
#13524=AXIS2_PLACEMENT_3D('',#18987,#15314,#15315);
#13525=AXIS2_PLACEMENT_3D('',#18990,#15317,#15318);
#13526=AXIS2_PLACEMENT_3D('',#18991,#15319,#15320);
#13527=AXIS2_PLACEMENT_3D('',#18993,#15321,#15322);
#13528=AXIS2_PLACEMENT_3D('',#18996,#15324,#15325);
#13529=AXIS2_PLACEMENT_3D('',#18997,#15326,#15327);
#13530=AXIS2_PLACEMENT_3D('',#18999,#15328,#15329);
#13531=AXIS2_PLACEMENT_3D('',#19002,#15331,#15332);
#13532=AXIS2_PLACEMENT_3D('',#19003,#15333,#15334);
#13533=AXIS2_PLACEMENT_3D('',#19005,#15335,#15336);
#13534=AXIS2_PLACEMENT_3D('',#19008,#15338,#15339);
#13535=AXIS2_PLACEMENT_3D('',#19009,#15340,#15341);
#13536=AXIS2_PLACEMENT_3D('',#19018,#15346,#15347);
#13537=AXIS2_PLACEMENT_3D('',#19027,#15352,#15353);
#13538=AXIS2_PLACEMENT_3D('',#19033,#15357,#15358);
#13539=AXIS2_PLACEMENT_3D('',#19039,#15362,#15363);
#13540=AXIS2_PLACEMENT_3D('',#19046,#15368,#15369);
#13541=AXIS2_PLACEMENT_3D('',#19050,#15372,#15373);
#13542=AXIS2_PLACEMENT_3D('',#19055,#15377,#15378);
#13543=AXIS2_PLACEMENT_3D('',#19057,#15380,#15381);
#13544=AXIS2_PLACEMENT_3D('',#19058,#15382,#15383);
#13545=AXIS2_PLACEMENT_3D('',#19059,#15384,#15385);
#13546=AXIS2_PLACEMENT_3D('',#19060,#15386,#15387);
#13547=AXIS2_PLACEMENT_3D('',#19062,#15388,#15389);
#13548=AXIS2_PLACEMENT_3D('',#19065,#15391,#15392);
#13549=AXIS2_PLACEMENT_3D('',#19066,#15393,#15394);
#13550=AXIS2_PLACEMENT_3D('',#19068,#15395,#15396);
#13551=AXIS2_PLACEMENT_3D('',#19071,#15398,#15399);
#13552=AXIS2_PLACEMENT_3D('',#19072,#15400,#15401);
#13553=AXIS2_PLACEMENT_3D('',#19074,#15402,#15403);
#13554=AXIS2_PLACEMENT_3D('',#19077,#15405,#15406);
#13555=AXIS2_PLACEMENT_3D('',#19078,#15407,#15408);
#13556=AXIS2_PLACEMENT_3D('',#19080,#15409,#15410);
#13557=AXIS2_PLACEMENT_3D('',#19083,#15412,#15413);
#13558=AXIS2_PLACEMENT_3D('',#19084,#15414,#15415);
#13559=AXIS2_PLACEMENT_3D('',#19086,#15416,#15417);
#13560=AXIS2_PLACEMENT_3D('',#19089,#15419,#15420);
#13561=AXIS2_PLACEMENT_3D('',#19090,#15421,#15422);
#13562=AXIS2_PLACEMENT_3D('',#19092,#15423,#15424);
#13563=AXIS2_PLACEMENT_3D('',#19093,#15425,#15426);
#13564=AXIS2_PLACEMENT_3D('',#19096,#15428,#15429);
#13565=AXIS2_PLACEMENT_3D('',#19097,#15430,#15431);
#13566=AXIS2_PLACEMENT_3D('',#19099,#15432,#15433);
#13567=AXIS2_PLACEMENT_3D('',#19102,#15435,#15436);
#13568=AXIS2_PLACEMENT_3D('',#19103,#15437,#15438);
#13569=AXIS2_PLACEMENT_3D('',#19104,#15439,#15440);
#13570=AXIS2_PLACEMENT_3D('',#19105,#15441,#15442);
#13571=AXIS2_PLACEMENT_3D('',#19106,#15443,#15444);
#13572=AXIS2_PLACEMENT_3D('',#19108,#15445,#15446);
#13573=AXIS2_PLACEMENT_3D('',#19111,#15448,#15449);
#13574=AXIS2_PLACEMENT_3D('',#19112,#15450,#15451);
#13575=AXIS2_PLACEMENT_3D('',#19114,#15452,#15453);
#13576=AXIS2_PLACEMENT_3D('',#19117,#15455,#15456);
#13577=AXIS2_PLACEMENT_3D('',#19118,#15457,#15458);
#13578=AXIS2_PLACEMENT_3D('',#19120,#15459,#15460);
#13579=AXIS2_PLACEMENT_3D('',#19123,#15462,#15463);
#13580=AXIS2_PLACEMENT_3D('',#19124,#15464,#15465);
#13581=AXIS2_PLACEMENT_3D('',#19126,#15466,#15467);
#13582=AXIS2_PLACEMENT_3D('',#19129,#15469,#15470);
#13583=AXIS2_PLACEMENT_3D('',#19130,#15471,#15472);
#13584=AXIS2_PLACEMENT_3D('',#19132,#15473,#15474);
#13585=AXIS2_PLACEMENT_3D('',#19135,#15476,#15477);
#13586=AXIS2_PLACEMENT_3D('',#19136,#15478,#15479);
#13587=AXIS2_PLACEMENT_3D('',#19138,#15480,#15481);
#13588=AXIS2_PLACEMENT_3D('',#19139,#15482,#15483);
#13589=AXIS2_PLACEMENT_3D('',#19141,#15484,#15485);
#13590=AXIS2_PLACEMENT_3D('',#19143,#15487,#15488);
#13591=AXIS2_PLACEMENT_3D('',#19145,#15489,#15490);
#13592=AXIS2_PLACEMENT_3D('',#19148,#15492,#15493);
#13593=AXIS2_PLACEMENT_3D('',#19149,#15494,#15495);
#13594=AXIS2_PLACEMENT_3D('',#19150,#15496,#15497);
#13595=AXIS2_PLACEMENT_3D('',#19151,#15498,#15499);
#13596=AXIS2_PLACEMENT_3D('',#19152,#15500,#15501);
#13597=AXIS2_PLACEMENT_3D('',#19154,#15502,#15503);
#13598=AXIS2_PLACEMENT_3D('',#19155,#15504,#15505);
#13599=AXIS2_PLACEMENT_3D('',#19157,#15506,#15507);
#13600=AXIS2_PLACEMENT_3D('',#19160,#15509,#15510);
#13601=AXIS2_PLACEMENT_3D('',#19161,#15511,#15512);
#13602=AXIS2_PLACEMENT_3D('',#19163,#15514,#15515);
#13603=AXIS2_PLACEMENT_3D('',#19164,#15516,#15517);
#13604=AXIS2_PLACEMENT_3D('',#19165,#15518,#15519);
#13605=AXIS2_PLACEMENT_3D('',#19166,#15520,#15521);
#13606=AXIS2_PLACEMENT_3D('',#19169,#15522,#15523);
#13607=AXIS2_PLACEMENT_3D('',#19170,#15524,#15525);
#13608=AXIS2_PLACEMENT_3D('',#19172,#15526,#15527);
#13609=AXIS2_PLACEMENT_3D('',#19174,#15528,#15529);
#13610=AXIS2_PLACEMENT_3D('',#19175,#15530,#15531);
#13611=AXIS2_PLACEMENT_3D('',#19176,#15532,#15533);
#13612=AXIS2_PLACEMENT_3D('',#19179,#15535,#15536);
#13613=AXIS2_PLACEMENT_3D('',#19180,#15537,#15538);
#13614=AXIS2_PLACEMENT_3D('',#19182,#15539,#15540);
#13615=AXIS2_PLACEMENT_3D('',#19185,#15542,#15543);
#13616=AXIS2_PLACEMENT_3D('',#19186,#15544,#15545);
#13617=AXIS2_PLACEMENT_3D('',#19189,#15547,#15548);
#13618=AXIS2_PLACEMENT_3D('',#19190,#15549,#15550);
#13619=AXIS2_PLACEMENT_3D('',#19191,#15551,#15552);
#13620=AXIS2_PLACEMENT_3D('',#19193,#15553,#15554);
#13621=AXIS2_PLACEMENT_3D('',#19195,#15556,#15557);
#13622=AXIS2_PLACEMENT_3D('',#19197,#15558,#15559);
#13623=AXIS2_PLACEMENT_3D('',#19198,#15560,#15561);
#13624=AXIS2_PLACEMENT_3D('',#19200,#15563,#15564);
#13625=AXIS2_PLACEMENT_3D('',#19201,#15565,#15566);
#13626=AXIS2_PLACEMENT_3D('',#19204,#15567,#15568);
#13627=AXIS2_PLACEMENT_3D('',#19205,#15569,#15570);
#13628=AXIS2_PLACEMENT_3D('',#19207,#15571,#15572);
#13629=AXIS2_PLACEMENT_3D('',#19209,#15573,#15574);
#13630=AXIS2_PLACEMENT_3D('',#19210,#15575,#15576);
#13631=AXIS2_PLACEMENT_3D('',#19211,#15577,#15578);
#13632=AXIS2_PLACEMENT_3D('',#19213,#15579,#15580);
#13633=AXIS2_PLACEMENT_3D('',#19215,#15582,#15583);
#13634=AXIS2_PLACEMENT_3D('',#19217,#15584,#15585);
#13635=AXIS2_PLACEMENT_3D('',#19219,#15586,#15587);
#13636=AXIS2_PLACEMENT_3D('',#19220,#15588,#15589);
#13637=AXIS2_PLACEMENT_3D('',#19222,#15590,#15591);
#13638=AXIS2_PLACEMENT_3D('',#19224,#15593,#15594);
#13639=AXIS2_PLACEMENT_3D('',#19226,#15595,#15596);
#13640=AXIS2_PLACEMENT_3D('',#19228,#15598,#15599);
#13641=AXIS2_PLACEMENT_3D('',#19230,#15600,#15601);
#13642=AXIS2_PLACEMENT_3D('',#19232,#15603,#15604);
#13643=AXIS2_PLACEMENT_3D('',#19233,#15605,#15606);
#13644=AXIS2_PLACEMENT_3D('',#19235,#15608,#15609);
#13645=AXIS2_PLACEMENT_3D('',#19236,#15610,#15611);
#13646=AXIS2_PLACEMENT_3D('',#19239,#15612,#15613);
#13647=AXIS2_PLACEMENT_3D('',#19240,#15614,#15615);
#13648=AXIS2_PLACEMENT_3D('',#19243,#15616,#15617);
#13649=AXIS2_PLACEMENT_3D('',#19244,#15618,#15619);
#13650=AXIS2_PLACEMENT_3D('',#19247,#15620,#15621);
#13651=AXIS2_PLACEMENT_3D('',#19248,#15622,#15623);
#13652=AXIS2_PLACEMENT_3D('',#19251,#15624,#15625);
#13653=AXIS2_PLACEMENT_3D('',#19252,#15626,#15627);
#13654=AXIS2_PLACEMENT_3D('',#19255,#15628,#15629);
#13655=AXIS2_PLACEMENT_3D('',#19256,#15630,#15631);
#13656=AXIS2_PLACEMENT_3D('',#19259,#15632,#15633);
#13657=AXIS2_PLACEMENT_3D('',#19260,#15634,#15635);
#13658=AXIS2_PLACEMENT_3D('',#19263,#15636,#15637);
#13659=AXIS2_PLACEMENT_3D('',#19264,#15638,#15639);
#13660=AXIS2_PLACEMENT_3D('',#19265,#15640,#15641);
#13661=AXIS2_PLACEMENT_3D('',#19291,#15642,#15643);
#13662=AXIS2_PLACEMENT_3D('',#19315,#15644,#15645);
#13663=AXIS2_PLACEMENT_3D('',#19316,#15646,#15647);
#13664=AXIS2_PLACEMENT_3D('',#19318,#15648,#15649);
#13665=AXIS2_PLACEMENT_3D('',#19343,#15650,#15651);
#13666=AXIS2_PLACEMENT_3D('',#19368,#15652,#15653);
#13667=AXIS2_PLACEMENT_3D('',#19371,#15655,#15656);
#13668=AXIS2_PLACEMENT_3D('',#19373,#15657,#15658);
#13669=AXIS2_PLACEMENT_3D('',#19398,#15659,#15660);
#13670=AXIS2_PLACEMENT_3D('',#19423,#15661,#15662);
#13671=AXIS2_PLACEMENT_3D('',#19448,#15663,#15664);
#13672=AXIS2_PLACEMENT_3D('',#19472,#15665,#15666);
#13673=AXIS2_PLACEMENT_3D('',#19473,#15667,#15668);
#13674=AXIS2_PLACEMENT_3D('',#19475,#15669,#15670);
#13675=AXIS2_PLACEMENT_3D('',#19476,#15671,#15672);
#13676=AXIS2_PLACEMENT_3D('',#19477,#15673,#15674);
#13677=AXIS2_PLACEMENT_3D('',#19501,#15675,#15676);
#13678=AXIS2_PLACEMENT_3D('',#19502,#15677,#15678);
#13679=AXIS2_PLACEMENT_3D('',#19504,#15679,#15680);
#13680=AXIS2_PLACEMENT_3D('',#19505,#15681,#15682);
#13681=AXIS2_PLACEMENT_3D('',#19506,#15683,#15684);
#13682=AXIS2_PLACEMENT_3D('',#19530,#15685,#15686);
#13683=AXIS2_PLACEMENT_3D('',#19531,#15687,#15688);
#13684=AXIS2_PLACEMENT_3D('',#19533,#15689,#15690);
#13685=AXIS2_PLACEMENT_3D('',#19535,#15691,#15692);
#13686=AXIS2_PLACEMENT_3D('',#19536,#15693,#15694);
#13687=AXIS2_PLACEMENT_3D('',#19537,#15695,#15696);
#13688=AXIS2_PLACEMENT_3D('',#19561,#15697,#15698);
#13689=AXIS2_PLACEMENT_3D('',#19562,#15699,#15700);
#13690=AXIS2_PLACEMENT_3D('',#19564,#15701,#15702);
#13691=AXIS2_PLACEMENT_3D('',#19565,#15703,#15704);
#13692=AXIS2_PLACEMENT_3D('',#19566,#15705,#15706);
#13693=AXIS2_PLACEMENT_3D('',#19590,#15707,#15708);
#13694=AXIS2_PLACEMENT_3D('',#19591,#15709,#15710);
#13695=AXIS2_PLACEMENT_3D('',#19593,#15711,#15712);
#13696=AXIS2_PLACEMENT_3D('',#19594,#15713,#15714);
#13697=AXIS2_PLACEMENT_3D('',#19595,#15715,#15716);
#13698=AXIS2_PLACEMENT_3D('',#19619,#15717,#15718);
#13699=AXIS2_PLACEMENT_3D('',#19620,#15719,#15720);
#13700=AXIS2_PLACEMENT_3D('',#19622,#15721,#15722);
#13701=AXIS2_PLACEMENT_3D('',#19625,#15724,#15725);
#13702=AXIS2_PLACEMENT_3D('',#19649,#15726,#15727);
#13703=AXIS2_PLACEMENT_3D('',#19650,#15728,#15729);
#13704=AXIS2_PLACEMENT_3D('',#19651,#15730,#15731);
#13705=AXIS2_PLACEMENT_3D('',#19652,#15732,#15733);
#13706=AXIS2_PLACEMENT_3D('',#19653,#15734,#15735);
#13707=AXIS2_PLACEMENT_3D('',#19654,#15736,#15737);
#13708=AXIS2_PLACEMENT_3D('',#19655,#15738,#15739);
#13709=AXIS2_PLACEMENT_3D('',#19656,#15740,#15741);
#13710=AXIS2_PLACEMENT_3D('',#19657,#15742,#15743);
#13711=AXIS2_PLACEMENT_3D('',#19659,#15744,#15745);
#13712=AXIS2_PLACEMENT_3D('',#19661,#15746,#15747);
#13713=AXIS2_PLACEMENT_3D('',#19662,#15748,#15749);
#13714=AXIS2_PLACEMENT_3D('',#19664,#15750,#15751);
#13715=AXIS2_PLACEMENT_3D('',#19666,#15753,#15754);
#13716=AXIS2_PLACEMENT_3D('',#19668,#15755,#15756);
#13717=AXIS2_PLACEMENT_3D('',#19669,#15757,#15758);
#13718=AXIS2_PLACEMENT_3D('',#19671,#15760,#15761);
#13719=AXIS2_PLACEMENT_3D('',#19673,#15762,#15763);
#13720=AXIS2_PLACEMENT_3D('',#19675,#15764,#15765);
#13721=AXIS2_PLACEMENT_3D('',#19676,#15766,#15767);
#13722=AXIS2_PLACEMENT_3D('',#19678,#15768,#15769);
#13723=AXIS2_PLACEMENT_3D('',#19680,#15771,#15772);
#13724=AXIS2_PLACEMENT_3D('',#19682,#15773,#15774);
#13725=AXIS2_PLACEMENT_3D('',#19683,#15775,#15776);
#13726=AXIS2_PLACEMENT_3D('',#19685,#15778,#15779);
#13727=AXIS2_PLACEMENT_3D('',#19686,#15780,#15781);
#13728=AXIS2_PLACEMENT_3D('',#19687,#15782,#15783);
#13729=AXIS2_PLACEMENT_3D('',#19688,#15784,#15785);
#13730=AXIS2_PLACEMENT_3D('',#19689,#15786,#15787);
#13731=AXIS2_PLACEMENT_3D('',#19690,#15788,#15789);
#13732=AXIS2_PLACEMENT_3D('',#19691,#15790,#15791);
#13733=AXIS2_PLACEMENT_3D('',#19700,#15796,#15797);
#13734=AXIS2_PLACEMENT_3D('',#19706,#15801,#15802);
#13735=AXIS2_PLACEMENT_3D('',#19712,#15806,#15807);
#13736=AXIS2_PLACEMENT_3D('',#19718,#15811,#15812);
#13737=AXIS2_PLACEMENT_3D('',#19724,#15816,#15817);
#13738=AXIS2_PLACEMENT_3D('',#19727,#15820,#15821);
#13739=AXIS2_PLACEMENT_3D('',#19728,#15822,#15823);
#13740=AXIS2_PLACEMENT_3D('',#19729,#15824,#15825);
#13741=AXIS2_PLACEMENT_3D('',#19731,#15826,#15827);
#13742=AXIS2_PLACEMENT_3D('',#19732,#15828,#15829);
#13743=AXIS2_PLACEMENT_3D('',#19734,#15830,#15831);
#13744=AXIS2_PLACEMENT_3D('',#19735,#15832,#15833);
#13745=AXIS2_PLACEMENT_3D('',#19737,#15834,#15835);
#13746=AXIS2_PLACEMENT_3D('',#19739,#15837,#15838);
#13747=AXIS2_PLACEMENT_3D('',#19741,#15839,#15840);
#13748=AXIS2_PLACEMENT_3D('',#19743,#15842,#15843);
#13749=AXIS2_PLACEMENT_3D('',#19745,#15844,#15845);
#13750=AXIS2_PLACEMENT_3D('',#19747,#15847,#15848);
#13751=AXIS2_PLACEMENT_3D('',#19749,#15849,#15850);
#13752=AXIS2_PLACEMENT_3D('',#19750,#15851,#15852);
#13753=AXIS2_PLACEMENT_3D('',#19752,#15853,#15854);
#13754=AXIS2_PLACEMENT_3D('',#19754,#15856,#15857);
#13755=AXIS2_PLACEMENT_3D('',#19756,#15859,#15860);
#13756=AXIS2_PLACEMENT_3D('',#19757,#15861,#15862);
#13757=AXIS2_PLACEMENT_3D('',#19758,#15863,#15864);
#13758=AXIS2_PLACEMENT_3D('',#19760,#15865,#15866);
#13759=AXIS2_PLACEMENT_3D('',#19763,#15868,#15869);
#13760=AXIS2_PLACEMENT_3D('',#19764,#15870,#15871);
#13761=AXIS2_PLACEMENT_3D('',#19765,#15872,#15873);
#13762=AXIS2_PLACEMENT_3D('',#19774,#15878,#15879);
#13763=AXIS2_PLACEMENT_3D('',#19783,#15884,#15885);
#13764=AXIS2_PLACEMENT_3D('',#19785,#15886,#15887);
#13765=AXIS2_PLACEMENT_3D('',#19791,#15891,#15892);
#13766=AXIS2_PLACEMENT_3D('',#19792,#15893,#15894);
#13767=AXIS2_PLACEMENT_3D('',#19794,#15895,#15896);
#13768=AXIS2_PLACEMENT_3D('',#19800,#15900,#15901);
#13769=AXIS2_PLACEMENT_3D('',#19801,#15902,#15903);
#13770=AXIS2_PLACEMENT_3D('',#19807,#15907,#15908);
#13771=AXIS2_PLACEMENT_3D('',#19813,#15912,#15913);
#13772=AXIS2_PLACEMENT_3D('',#19819,#15917,#15918);
#13773=AXIS2_PLACEMENT_3D('',#19825,#15922,#15923);
#13774=AXIS2_PLACEMENT_3D('',#19831,#15927,#15928);
#13775=AXIS2_PLACEMENT_3D('',#19837,#15932,#15933);
#13776=AXIS2_PLACEMENT_3D('',#19843,#15937,#15938);
#13777=AXIS2_PLACEMENT_3D('',#19849,#15942,#15943);
#13778=AXIS2_PLACEMENT_3D('',#19855,#15947,#15948);
#13779=AXIS2_PLACEMENT_3D('',#19861,#15952,#15953);
#13780=AXIS2_PLACEMENT_3D('',#19867,#15957,#15958);
#13781=AXIS2_PLACEMENT_3D('',#19873,#15962,#15963);
#13782=AXIS2_PLACEMENT_3D('',#19879,#15967,#15968);
#13783=AXIS2_PLACEMENT_3D('',#19885,#15972,#15973);
#13784=AXIS2_PLACEMENT_3D('',#19891,#15977,#15978);
#13785=AXIS2_PLACEMENT_3D('',#19897,#15982,#15983);
#13786=AXIS2_PLACEMENT_3D('',#19903,#15987,#15988);
#13787=AXIS2_PLACEMENT_3D('',#19909,#15992,#15993);
#13788=AXIS2_PLACEMENT_3D('',#19915,#15997,#15998);
#13789=AXIS2_PLACEMENT_3D('',#19921,#16002,#16003);
#13790=AXIS2_PLACEMENT_3D('',#19927,#16007,#16008);
#13791=AXIS2_PLACEMENT_3D('',#19933,#16012,#16013);
#13792=AXIS2_PLACEMENT_3D('',#19939,#16017,#16018);
#13793=AXIS2_PLACEMENT_3D('',#19945,#16022,#16023);
#13794=AXIS2_PLACEMENT_3D('',#19951,#16027,#16028);
#13795=AXIS2_PLACEMENT_3D('',#19957,#16032,#16033);
#13796=AXIS2_PLACEMENT_3D('',#19963,#16037,#16038);
#13797=AXIS2_PLACEMENT_3D('',#19969,#16042,#16043);
#13798=AXIS2_PLACEMENT_3D('',#19975,#16047,#16048);
#13799=AXIS2_PLACEMENT_3D('',#19981,#16052,#16053);
#13800=AXIS2_PLACEMENT_3D('',#19987,#16057,#16058);
#13801=AXIS2_PLACEMENT_3D('',#19993,#16062,#16063);
#13802=AXIS2_PLACEMENT_3D('',#19999,#16067,#16068);
#13803=AXIS2_PLACEMENT_3D('',#20005,#16072,#16073);
#13804=AXIS2_PLACEMENT_3D('',#20011,#16077,#16078);
#13805=AXIS2_PLACEMENT_3D('',#20017,#16082,#16083);
#13806=AXIS2_PLACEMENT_3D('',#20023,#16087,#16088);
#13807=AXIS2_PLACEMENT_3D('',#20029,#16092,#16093);
#13808=AXIS2_PLACEMENT_3D('',#20035,#16097,#16098);
#13809=AXIS2_PLACEMENT_3D('',#20041,#16102,#16103);
#13810=AXIS2_PLACEMENT_3D('',#20047,#16107,#16108);
#13811=AXIS2_PLACEMENT_3D('',#20053,#16112,#16113);
#13812=AXIS2_PLACEMENT_3D('',#20059,#16117,#16118);
#13813=AXIS2_PLACEMENT_3D('',#20065,#16122,#16123);
#13814=AXIS2_PLACEMENT_3D('',#20071,#16127,#16128);
#13815=AXIS2_PLACEMENT_3D('',#20077,#16132,#16133);
#13816=AXIS2_PLACEMENT_3D('',#20083,#16137,#16138);
#13817=AXIS2_PLACEMENT_3D('',#20089,#16142,#16143);
#13818=AXIS2_PLACEMENT_3D('',#20095,#16147,#16148);
#13819=AXIS2_PLACEMENT_3D('',#20101,#16152,#16153);
#13820=AXIS2_PLACEMENT_3D('',#20107,#16157,#16158);
#13821=AXIS2_PLACEMENT_3D('',#20113,#16162,#16163);
#13822=AXIS2_PLACEMENT_3D('',#20119,#16167,#16168);
#13823=AXIS2_PLACEMENT_3D('',#20125,#16172,#16173);
#13824=AXIS2_PLACEMENT_3D('',#20131,#16177,#16178);
#13825=AXIS2_PLACEMENT_3D('',#20137,#16182,#16183);
#13826=AXIS2_PLACEMENT_3D('',#20143,#16187,#16188);
#13827=AXIS2_PLACEMENT_3D('',#20149,#16192,#16193);
#13828=AXIS2_PLACEMENT_3D('',#20155,#16197,#16198);
#13829=AXIS2_PLACEMENT_3D('',#20161,#16202,#16203);
#13830=AXIS2_PLACEMENT_3D('',#20167,#16207,#16208);
#13831=AXIS2_PLACEMENT_3D('',#20173,#16212,#16213);
#13832=AXIS2_PLACEMENT_3D('',#20179,#16217,#16218);
#13833=AXIS2_PLACEMENT_3D('',#20185,#16222,#16223);
#13834=AXIS2_PLACEMENT_3D('',#20191,#16227,#16228);
#13835=AXIS2_PLACEMENT_3D('',#20197,#16232,#16233);
#13836=AXIS2_PLACEMENT_3D('',#20203,#16237,#16238);
#13837=AXIS2_PLACEMENT_3D('',#20209,#16242,#16243);
#13838=AXIS2_PLACEMENT_3D('',#20215,#16247,#16248);
#13839=AXIS2_PLACEMENT_3D('',#20221,#16252,#16253);
#13840=AXIS2_PLACEMENT_3D('',#20227,#16257,#16258);
#13841=AXIS2_PLACEMENT_3D('',#20233,#16262,#16263);
#13842=AXIS2_PLACEMENT_3D('',#20239,#16267,#16268);
#13843=AXIS2_PLACEMENT_3D('',#20245,#16272,#16273);
#13844=AXIS2_PLACEMENT_3D('',#20251,#16277,#16278);
#13845=AXIS2_PLACEMENT_3D('',#20257,#16282,#16283);
#13846=AXIS2_PLACEMENT_3D('',#20263,#16287,#16288);
#13847=AXIS2_PLACEMENT_3D('',#20269,#16292,#16293);
#13848=AXIS2_PLACEMENT_3D('',#20275,#16297,#16298);
#13849=AXIS2_PLACEMENT_3D('',#20281,#16302,#16303);
#13850=AXIS2_PLACEMENT_3D('',#20287,#16307,#16308);
#13851=AXIS2_PLACEMENT_3D('',#20293,#16312,#16313);
#13852=AXIS2_PLACEMENT_3D('',#20299,#16317,#16318);
#13853=AXIS2_PLACEMENT_3D('',#20305,#16322,#16323);
#13854=AXIS2_PLACEMENT_3D('',#20311,#16327,#16328);
#13855=AXIS2_PLACEMENT_3D('',#20317,#16332,#16333);
#13856=AXIS2_PLACEMENT_3D('',#20323,#16337,#16338);
#13857=AXIS2_PLACEMENT_3D('',#20329,#16342,#16343);
#13858=AXIS2_PLACEMENT_3D('',#20335,#16347,#16348);
#13859=AXIS2_PLACEMENT_3D('',#20341,#16352,#16353);
#13860=AXIS2_PLACEMENT_3D('',#20347,#16357,#16358);
#13861=AXIS2_PLACEMENT_3D('',#20353,#16362,#16363);
#13862=AXIS2_PLACEMENT_3D('',#20359,#16367,#16368);
#13863=AXIS2_PLACEMENT_3D('',#20365,#16372,#16373);
#13864=AXIS2_PLACEMENT_3D('',#20371,#16377,#16378);
#13865=AXIS2_PLACEMENT_3D('',#20377,#16382,#16383);
#13866=AXIS2_PLACEMENT_3D('',#20383,#16387,#16388);
#13867=AXIS2_PLACEMENT_3D('',#20389,#16392,#16393);
#13868=AXIS2_PLACEMENT_3D('',#20395,#16397,#16398);
#13869=AXIS2_PLACEMENT_3D('',#20401,#16402,#16403);
#13870=AXIS2_PLACEMENT_3D('',#20407,#16407,#16408);
#13871=AXIS2_PLACEMENT_3D('',#20413,#16412,#16413);
#13872=AXIS2_PLACEMENT_3D('',#20419,#16417,#16418);
#13873=AXIS2_PLACEMENT_3D('',#20425,#16422,#16423);
#13874=AXIS2_PLACEMENT_3D('',#20431,#16427,#16428);
#13875=AXIS2_PLACEMENT_3D('',#20437,#16432,#16433);
#13876=AXIS2_PLACEMENT_3D('',#20443,#16437,#16438);
#13877=AXIS2_PLACEMENT_3D('',#20449,#16442,#16443);
#13878=AXIS2_PLACEMENT_3D('',#20455,#16447,#16448);
#13879=AXIS2_PLACEMENT_3D('',#20461,#16452,#16453);
#13880=AXIS2_PLACEMENT_3D('',#20467,#16457,#16458);
#13881=AXIS2_PLACEMENT_3D('',#20473,#16462,#16463);
#13882=AXIS2_PLACEMENT_3D('',#20479,#16467,#16468);
#13883=AXIS2_PLACEMENT_3D('',#20485,#16472,#16473);
#13884=AXIS2_PLACEMENT_3D('',#20491,#16477,#16478);
#13885=AXIS2_PLACEMENT_3D('',#20497,#16482,#16483);
#13886=AXIS2_PLACEMENT_3D('',#20503,#16487,#16488);
#13887=AXIS2_PLACEMENT_3D('',#20509,#16492,#16493);
#13888=AXIS2_PLACEMENT_3D('',#20515,#16497,#16498);
#13889=AXIS2_PLACEMENT_3D('',#20521,#16502,#16503);
#13890=AXIS2_PLACEMENT_3D('',#20527,#16507,#16508);
#13891=AXIS2_PLACEMENT_3D('',#20533,#16512,#16513);
#13892=AXIS2_PLACEMENT_3D('',#20539,#16517,#16518);
#13893=AXIS2_PLACEMENT_3D('',#20545,#16522,#16523);
#13894=AXIS2_PLACEMENT_3D('',#20551,#16527,#16528);
#13895=AXIS2_PLACEMENT_3D('',#20557,#16532,#16533);
#13896=AXIS2_PLACEMENT_3D('',#20563,#16537,#16538);
#13897=AXIS2_PLACEMENT_3D('',#20569,#16542,#16543);
#13898=AXIS2_PLACEMENT_3D('',#20575,#16547,#16548);
#13899=AXIS2_PLACEMENT_3D('',#20581,#16552,#16553);
#13900=AXIS2_PLACEMENT_3D('',#20587,#16557,#16558);
#13901=AXIS2_PLACEMENT_3D('',#20593,#16562,#16563);
#13902=AXIS2_PLACEMENT_3D('',#20599,#16567,#16568);
#13903=AXIS2_PLACEMENT_3D('',#20605,#16572,#16573);
#13904=AXIS2_PLACEMENT_3D('',#20611,#16577,#16578);
#13905=AXIS2_PLACEMENT_3D('',#20617,#16582,#16583);
#13906=AXIS2_PLACEMENT_3D('',#20623,#16587,#16588);
#13907=AXIS2_PLACEMENT_3D('',#20629,#16592,#16593);
#13908=AXIS2_PLACEMENT_3D('',#20635,#16597,#16598);
#13909=AXIS2_PLACEMENT_3D('',#20641,#16602,#16603);
#13910=AXIS2_PLACEMENT_3D('',#20647,#16607,#16608);
#13911=AXIS2_PLACEMENT_3D('',#20653,#16612,#16613);
#13912=AXIS2_PLACEMENT_3D('',#20659,#16617,#16618);
#13913=AXIS2_PLACEMENT_3D('',#20665,#16622,#16623);
#13914=AXIS2_PLACEMENT_3D('',#20671,#16627,#16628);
#13915=AXIS2_PLACEMENT_3D('',#20677,#16632,#16633);
#13916=AXIS2_PLACEMENT_3D('',#20683,#16637,#16638);
#13917=AXIS2_PLACEMENT_3D('',#20689,#16642,#16643);
#13918=AXIS2_PLACEMENT_3D('',#20695,#16647,#16648);
#13919=AXIS2_PLACEMENT_3D('',#20701,#16652,#16653);
#13920=AXIS2_PLACEMENT_3D('',#20707,#16657,#16658);
#13921=AXIS2_PLACEMENT_3D('',#20713,#16662,#16663);
#13922=AXIS2_PLACEMENT_3D('',#20719,#16667,#16668);
#13923=AXIS2_PLACEMENT_3D('',#20725,#16672,#16673);
#13924=AXIS2_PLACEMENT_3D('',#20731,#16677,#16678);
#13925=AXIS2_PLACEMENT_3D('',#20737,#16682,#16683);
#13926=AXIS2_PLACEMENT_3D('',#20743,#16687,#16688);
#13927=AXIS2_PLACEMENT_3D('',#20749,#16692,#16693);
#13928=AXIS2_PLACEMENT_3D('',#20755,#16697,#16698);
#13929=AXIS2_PLACEMENT_3D('',#20761,#16702,#16703);
#13930=AXIS2_PLACEMENT_3D('',#20764,#16706,#16707);
#13931=AXIS2_PLACEMENT_3D('',#20765,#16708,#16709);
#13932=AXIS2_PLACEMENT_3D('',#20766,#16710,#16711);
#13933=AXIS2_PLACEMENT_3D('',#20768,#16712,#16713);
#13934=AXIS2_PLACEMENT_3D('',#20772,#16716,#16717);
#13935=AXIS2_PLACEMENT_3D('',#20773,#16718,#16719);
#13936=AXIS2_PLACEMENT_3D('',#20774,#16720,#16721);
#13937=AXIS2_PLACEMENT_3D('',#20775,#16722,#16723);
#13938=AXIS2_PLACEMENT_3D('',#20776,#16724,#16725);
#13939=AXIS2_PLACEMENT_3D('',#20780,#16727,#16728);
#13940=AXIS2_PLACEMENT_3D('',#20781,#16729,#16730);
#13941=AXIS2_PLACEMENT_3D('',#20794,#16731,#16732);
#13942=AXIS2_PLACEMENT_3D('',#20847,#16734,#16735);
#13943=AXIS2_PLACEMENT_3D('',#20849,#16737,#16738);
#13944=AXIS2_PLACEMENT_3D('',#20851,#16739,#16740);
#13945=AXIS2_PLACEMENT_3D('',#20854,#16742,#16743);
#13946=AXIS2_PLACEMENT_3D('',#20855,#16744,#16745);
#13947=AXIS2_PLACEMENT_3D('',#20857,#16746,#16747);
#13948=AXIS2_PLACEMENT_3D('',#20860,#16749,#16750);
#13949=AXIS2_PLACEMENT_3D('',#20861,#16751,#16752);
#13950=AXIS2_PLACEMENT_3D('',#20862,#16753,#16754);
#13951=AXIS2_PLACEMENT_3D('',#20864,#16755,#16756);
#13952=AXIS2_PLACEMENT_3D('',#20867,#16758,#16759);
#13953=AXIS2_PLACEMENT_3D('',#20868,#16760,#16761);
#13954=AXIS2_PLACEMENT_3D('',#20869,#16762,#16763);
#13955=AXIS2_PLACEMENT_3D('',#20870,#16764,#16765);
#13956=AXIS2_PLACEMENT_3D('',#20871,#16766,#16767);
#13957=AXIS2_PLACEMENT_3D('',#20873,#16768,#16769);
#13958=AXIS2_PLACEMENT_3D('',#20876,#16771,#16772);
#13959=AXIS2_PLACEMENT_3D('',#20877,#16773,#16774);
#13960=AXIS2_PLACEMENT_3D('',#20878,#16775,#16776);
#13961=AXIS2_PLACEMENT_3D('',#20879,#16777,#16778);
#13962=AXIS2_PLACEMENT_3D('',#20880,#16779,#16780);
#13963=AXIS2_PLACEMENT_3D('',#20882,#16781,#16782);
#13964=AXIS2_PLACEMENT_3D('',#20885,#16784,#16785);
#13965=AXIS2_PLACEMENT_3D('',#20886,#16786,#16787);
#13966=AXIS2_PLACEMENT_3D('',#20887,#16788,#16789);
#13967=AXIS2_PLACEMENT_3D('',#20888,#16790,#16791);
#13968=AXIS2_PLACEMENT_3D('',#20889,#16792,#16793);
#13969=AXIS2_PLACEMENT_3D('',#20967,#16795,#16796);
#13970=AXIS2_PLACEMENT_3D('',#20976,#16801,#16802);
#13971=AXIS2_PLACEMENT_3D('',#20985,#16807,#16808);
#13972=AXIS2_PLACEMENT_3D('',#20991,#16812,#16813);
#13973=AXIS2_PLACEMENT_3D('',#20997,#16817,#16818);
#13974=AXIS2_PLACEMENT_3D('',#20998,#16819,#16820);
#13975=AXIS2_PLACEMENT_3D('',#20999,#16821,#16822);
#13976=AXIS2_PLACEMENT_3D('',#21000,#16823,#16824);
#13977=AXIS2_PLACEMENT_3D('',#21001,#16825,#16826);
#13978=AXIS2_PLACEMENT_3D('',#21002,#16827,#16828);
#13979=AXIS2_PLACEMENT_3D('',#21003,#16829,#16830);
#13980=AXIS2_PLACEMENT_3D('',#21004,#16831,#16832);
#13981=AXIS2_PLACEMENT_3D('',#21005,#16833,#16834);
#13982=AXIS2_PLACEMENT_3D('',#21006,#16835,#16836);
#13983=AXIS2_PLACEMENT_3D('',#21015,#16841,#16842);
#13984=AXIS2_PLACEMENT_3D('',#21021,#16846,#16847);
#13985=AXIS2_PLACEMENT_3D('',#21027,#16851,#16852);
#13986=AXIS2_PLACEMENT_3D('',#21033,#16856,#16857);
#13987=AXIS2_PLACEMENT_3D('',#21039,#16861,#16862);
#13988=AXIS2_PLACEMENT_3D('',#21042,#16865,#16866);
#13989=AXIS2_PLACEMENT_3D('',#21043,#16867,#16868);
#13990=AXIS2_PLACEMENT_3D('',#21045,#16869,#16870);
#13991=AXIS2_PLACEMENT_3D('',#21046,#16871,#16872);
#13992=AXIS2_PLACEMENT_3D('',#21048,#16873,#16874);
#13993=AXIS2_PLACEMENT_3D('',#21050,#16876,#16877);
#13994=AXIS2_PLACEMENT_3D('',#21052,#16878,#16879);
#13995=AXIS2_PLACEMENT_3D('',#21054,#16881,#16882);
#13996=AXIS2_PLACEMENT_3D('',#21056,#16883,#16884);
#13997=AXIS2_PLACEMENT_3D('',#21058,#16886,#16887);
#13998=AXIS2_PLACEMENT_3D('',#21059,#16888,#16889);
#13999=AXIS2_PLACEMENT_3D('',#21060,#16890,#16891);
#14000=AXIS2_PLACEMENT_3D('',#21061,#16892,#16893);
#14001=AXIS2_PLACEMENT_3D('',#21062,#16894,#16895);
#14002=AXIS2_PLACEMENT_3D('',#21063,#16896,#16897);
#14003=AXIS2_PLACEMENT_3D('',#21064,#16898,#16899);
#14004=AXIS2_PLACEMENT_3D('',#21065,#16900,#16901);
#14005=AXIS2_PLACEMENT_3D('',#21066,#16902,#16903);
#14006=AXIS2_PLACEMENT_3D('',#21067,#16904,#16905);
#14007=AXIS2_PLACEMENT_3D('',#21069,#16906,#16907);
#14008=AXIS2_PLACEMENT_3D('',#21072,#16909,#16910);
#14009=AXIS2_PLACEMENT_3D('',#21073,#16911,#16912);
#14010=AXIS2_PLACEMENT_3D('',#21074,#16913,#16914);
#14011=AXIS2_PLACEMENT_3D('',#21076,#16915,#16916);
#14012=AXIS2_PLACEMENT_3D('',#21079,#16918,#16919);
#14013=AXIS2_PLACEMENT_3D('',#21080,#16920,#16921);
#14014=AXIS2_PLACEMENT_3D('',#21081,#16922,#16923);
#14015=AXIS2_PLACEMENT_3D('',#21090,#16928,#16929);
#14016=AXIS2_PLACEMENT_3D('',#21092,#16930,#16931);
#14017=AXIS2_PLACEMENT_3D('',#21096,#16934,#16935);
#14018=AXIS2_PLACEMENT_3D('',#21100,#16938,#16939);
#14019=AXIS2_PLACEMENT_3D('',#21104,#16942,#16943);
#14020=AXIS2_PLACEMENT_3D('',#21105,#16944,#16945);
#14021=AXIS2_PLACEMENT_3D('',#21106,#16946,#16947);
#14022=AXIS2_PLACEMENT_3D('',#21115,#16952,#16953);
#14023=AXIS2_PLACEMENT_3D('',#21117,#16954,#16955);
#14024=AXIS2_PLACEMENT_3D('',#21121,#16958,#16959);
#14025=AXIS2_PLACEMENT_3D('',#21125,#16962,#16963);
#14026=AXIS2_PLACEMENT_3D('',#21129,#16966,#16967);
#14027=AXIS2_PLACEMENT_3D('',#21130,#16968,#16969);
#14028=AXIS2_PLACEMENT_3D('',#21131,#16970,#16971);
#14029=AXIS2_PLACEMENT_3D('',#21133,#16972,#16973);
#14030=AXIS2_PLACEMENT_3D('',#21136,#16975,#16976);
#14031=AXIS2_PLACEMENT_3D('',#21137,#16977,#16978);
#14032=AXIS2_PLACEMENT_3D('',#21138,#16979,#16980);
#14033=AXIS2_PLACEMENT_3D('',#21139,#16981,#16982);
#14034=AXIS2_PLACEMENT_3D('',#21140,#16983,#16984);
#14035=AXIS2_PLACEMENT_3D('',#21142,#16985,#16986);
#14036=AXIS2_PLACEMENT_3D('',#21145,#16988,#16989);
#14037=AXIS2_PLACEMENT_3D('',#21146,#16990,#16991);
#14038=AXIS2_PLACEMENT_3D('',#21148,#16992,#16993);
#14039=AXIS2_PLACEMENT_3D('',#21151,#16995,#16996);
#14040=AXIS2_PLACEMENT_3D('',#21152,#16997,#16998);
#14041=AXIS2_PLACEMENT_3D('',#21153,#16999,#17000);
#14042=AXIS2_PLACEMENT_3D('',#21154,#17001,#17002);
#14043=AXIS2_PLACEMENT_3D('',#21155,#17003,#17004);
#14044=AXIS2_PLACEMENT_3D('',#21157,#17005,#17006);
#14045=AXIS2_PLACEMENT_3D('',#21160,#17008,#17009);
#14046=AXIS2_PLACEMENT_3D('',#21161,#17010,#17011);
#14047=AXIS2_PLACEMENT_3D('',#21163,#17012,#17013);
#14048=AXIS2_PLACEMENT_3D('',#21166,#17015,#17016);
#14049=AXIS2_PLACEMENT_3D('',#21167,#17017,#17018);
#14050=AXIS2_PLACEMENT_3D('',#21168,#17019,#17020);
#14051=AXIS2_PLACEMENT_3D('',#21169,#17021,#17022);
#14052=AXIS2_PLACEMENT_3D('',#21170,#17023,#17024);
#14053=AXIS2_PLACEMENT_3D('',#21172,#17025,#17026);
#14054=AXIS2_PLACEMENT_3D('',#21175,#17028,#17029);
#14055=AXIS2_PLACEMENT_3D('',#21176,#17030,#17031);
#14056=AXIS2_PLACEMENT_3D('',#21178,#17032,#17033);
#14057=AXIS2_PLACEMENT_3D('',#21181,#17035,#17036);
#14058=AXIS2_PLACEMENT_3D('',#21182,#17037,#17038);
#14059=AXIS2_PLACEMENT_3D('',#21183,#17039,#17040);
#14060=AXIS2_PLACEMENT_3D('',#21184,#17041,#17042);
#14061=AXIS2_PLACEMENT_3D('',#21185,#17043,#17044);
#14062=AXIS2_PLACEMENT_3D('',#21187,#17045,#17046);
#14063=AXIS2_PLACEMENT_3D('',#21190,#17048,#17049);
#14064=AXIS2_PLACEMENT_3D('',#21191,#17050,#17051);
#14065=AXIS2_PLACEMENT_3D('',#21193,#17052,#17053);
#14066=AXIS2_PLACEMENT_3D('',#21196,#17055,#17056);
#14067=AXIS2_PLACEMENT_3D('',#21197,#17057,#17058);
#14068=AXIS2_PLACEMENT_3D('',#21198,#17059,#17060);
#14069=AXIS2_PLACEMENT_3D('',#21199,#17061,#17062);
#14070=AXIS2_PLACEMENT_3D('',#21200,#17063,#17064);
#14071=AXIS2_PLACEMENT_3D('',#21209,#17069,#17070);
#14072=AXIS2_PLACEMENT_3D('',#21215,#17074,#17075);
#14073=AXIS2_PLACEMENT_3D('',#21221,#17079,#17080);
#14074=AXIS2_PLACEMENT_3D('',#21224,#17083,#17084);
#14075=AXIS2_PLACEMENT_3D('',#21225,#17085,#17086);
#14076=AXIS2_PLACEMENT_3D('',#21226,#17087,#17088);
#14077=AXIS2_PLACEMENT_3D('',#21227,#17089,#17090);
#14078=AXIS2_PLACEMENT_3D('',#21236,#17095,#17096);
#14079=AXIS2_PLACEMENT_3D('',#21242,#17100,#17101);
#14080=AXIS2_PLACEMENT_3D('',#21248,#17105,#17106);
#14081=AXIS2_PLACEMENT_3D('',#21251,#17109,#17110);
#14082=AXIS2_PLACEMENT_3D('',#21252,#17111,#17112);
#14083=AXIS2_PLACEMENT_3D('',#21253,#17113,#17114);
#14084=AXIS2_PLACEMENT_3D('',#21254,#17115,#17116);
#14085=AXIS2_PLACEMENT_3D('',#21256,#17117,#17118);
#14086=AXIS2_PLACEMENT_3D('',#21259,#17120,#17121);
#14087=AXIS2_PLACEMENT_3D('',#21260,#17122,#17123);
#14088=AXIS2_PLACEMENT_3D('',#21269,#17128,#17129);
#14089=AXIS2_PLACEMENT_3D('',#21275,#17133,#17134);
#14090=AXIS2_PLACEMENT_3D('',#21281,#17138,#17139);
#14091=AXIS2_PLACEMENT_3D('',#21283,#17140,#17141);
#14092=AXIS2_PLACEMENT_3D('',#21284,#17142,#17143);
#14093=AXIS2_PLACEMENT_3D('',#21285,#17144,#17145);
#14094=AXIS2_PLACEMENT_3D('',#21286,#17146,#17147);
#14095=AXIS2_PLACEMENT_3D('',#21287,#17148,#17149);
#14096=AXIS2_PLACEMENT_3D('',#21292,#17151,#17152);
#14097=AXIS2_PLACEMENT_3D('',#21295,#17154,#17155);
#14098=AXIS2_PLACEMENT_3D('',#21296,#17156,#17157);
#14099=AXIS2_PLACEMENT_3D('',#21302,#17161,#17162);
#14100=AXIS2_PLACEMENT_3D('',#21305,#17164,#17165);
#14101=AXIS2_PLACEMENT_3D('',#21306,#17166,#17167);
#14102=AXIS2_PLACEMENT_3D('',#21310,#17170,#17171);
#14103=AXIS2_PLACEMENT_3D('',#21311,#17172,#17173);
#14104=AXIS2_PLACEMENT_3D('',#21312,#17174,#17175);
#14105=AXIS2_PLACEMENT_3D('',#21315,#17177,#17178);
#14106=AXIS2_PLACEMENT_3D('',#21316,#17179,#17180);
#14107=AXIS2_PLACEMENT_3D('',#21317,#17181,#17182);
#14108=AXIS2_PLACEMENT_3D('',#21318,#17183,#17184);
#14109=AXIS2_PLACEMENT_3D('',#21320,#17185,#17186);
#14110=AXIS2_PLACEMENT_3D('',#21323,#17188,#17189);
#14111=AXIS2_PLACEMENT_3D('',#21324,#17190,#17191);
#14112=AXIS2_PLACEMENT_3D('',#21326,#17192,#17193);
#14113=AXIS2_PLACEMENT_3D('',#21329,#17195,#17196);
#14114=AXIS2_PLACEMENT_3D('',#21330,#17197,#17198);
#14115=AXIS2_PLACEMENT_3D('',#21331,#17199,#17200);
#14116=AXIS2_PLACEMENT_3D('',#21332,#17201,#17202);
#14117=AXIS2_PLACEMENT_3D('',#21333,#17203,#17204);
#14118=AXIS2_PLACEMENT_3D('',#21335,#17205,#17206);
#14119=AXIS2_PLACEMENT_3D('',#21338,#17208,#17209);
#14120=AXIS2_PLACEMENT_3D('',#21339,#17210,#17211);
#14121=AXIS2_PLACEMENT_3D('',#21341,#17212,#17213);
#14122=AXIS2_PLACEMENT_3D('',#21344,#17215,#17216);
#14123=AXIS2_PLACEMENT_3D('',#21345,#17217,#17218);
#14124=AXIS2_PLACEMENT_3D('',#21346,#17219,#17220);
#14125=AXIS2_PLACEMENT_3D('',#21347,#17221,#17222);
#14126=AXIS2_PLACEMENT_3D('',#21348,#17223,#17224);
#14127=AXIS2_PLACEMENT_3D('',#21350,#17225,#17226);
#14128=AXIS2_PLACEMENT_3D('',#21353,#17228,#17229);
#14129=AXIS2_PLACEMENT_3D('',#21354,#17230,#17231);
#14130=AXIS2_PLACEMENT_3D('',#21356,#17232,#17233);
#14131=AXIS2_PLACEMENT_3D('',#21359,#17235,#17236);
#14132=AXIS2_PLACEMENT_3D('',#21360,#17237,#17238);
#14133=AXIS2_PLACEMENT_3D('',#21361,#17239,#17240);
#14134=AXIS2_PLACEMENT_3D('',#21362,#17241,#17242);
#14135=AXIS2_PLACEMENT_3D('',#21363,#17243,#17244);
#14136=AXIS2_PLACEMENT_3D('',#21372,#17249,#17250);
#14137=AXIS2_PLACEMENT_3D('',#21378,#17254,#17255);
#14138=AXIS2_PLACEMENT_3D('',#21384,#17259,#17260);
#14139=AXIS2_PLACEMENT_3D('',#21387,#17261,#17262);
#14140=AXIS2_PLACEMENT_3D('',#21533,#17264,#17265);
#14141=AXIS2_PLACEMENT_3D('',#21679,#17267,#17268);
#14142=AXIS2_PLACEMENT_3D('',#21825,#17270,#17271);
#14143=AXIS2_PLACEMENT_3D('',#21971,#17273,#17274);
#14144=AXIS2_PLACEMENT_3D('',#22117,#17276,#17277);
#14145=AXIS2_PLACEMENT_3D('',#22263,#17279,#17280);
#14146=AXIS2_PLACEMENT_3D('',#22409,#17282,#17283);
#14147=AXIS2_PLACEMENT_3D('',#22555,#17285,#17286);
#14148=AXIS2_PLACEMENT_3D('',#22701,#17288,#17289);
#14149=AXIS2_PLACEMENT_3D('',#22847,#17291,#17292);
#14150=AXIS2_PLACEMENT_3D('',#22993,#17294,#17295);
#14151=AXIS2_PLACEMENT_3D('',#23139,#17297,#17298);
#14152=AXIS2_PLACEMENT_3D('',#23285,#17300,#17301);
#14153=AXIS2_PLACEMENT_3D('',#23431,#17303,#17304);
#14154=AXIS2_PLACEMENT_3D('',#23577,#17306,#17307);
#14155=AXIS2_PLACEMENT_3D('',#23723,#17309,#17310);
#14156=AXIS2_PLACEMENT_3D('',#23869,#17312,#17313);
#14157=AXIS2_PLACEMENT_3D('',#24015,#17315,#17316);
#14158=AXIS2_PLACEMENT_3D('',#24161,#17318,#17319);
#14159=AXIS2_PLACEMENT_3D('',#24305,#17321,#17322);
#14160=AXIS2_PLACEMENT_3D('',#24306,#17323,#17324);
#14161=AXIS2_PLACEMENT_3D('',#24307,#17325,#17326);
#14162=AXIS2_PLACEMENT_3D('',#24308,#17327,#17328);
#14163=AXIS2_PLACEMENT_3D('',#24310,#17329,#17330);
#14164=AXIS2_PLACEMENT_3D('',#24313,#17332,#17333);
#14165=AXIS2_PLACEMENT_3D('',#24314,#17334,#17335);
#14166=AXIS2_PLACEMENT_3D('',#24529,#17338,#17339);
#14167=AXIS2_PLACEMENT_3D('',#24745,#17343,#17344);
#14168=AXIS2_PLACEMENT_3D('',#24747,#17345,#17346);
#14169=AXIS2_PLACEMENT_3D('',#24961,#17349,#17350);
#14170=AXIS2_PLACEMENT_3D('',#25177,#17354,#17355);
#14171=AXIS2_PLACEMENT_3D('',#25179,#17356,#17357);
#14172=AXIS2_PLACEMENT_3D('',#25393,#17360,#17361);
#14173=AXIS2_PLACEMENT_3D('',#25609,#17365,#17366);
#14174=AXIS2_PLACEMENT_3D('',#25611,#17367,#17368);
#14175=AXIS2_PLACEMENT_3D('',#25825,#17371,#17372);
#14176=AXIS2_PLACEMENT_3D('',#26041,#17376,#17377);
#14177=AXIS2_PLACEMENT_3D('',#26043,#17378,#17379);
#14178=AXIS2_PLACEMENT_3D('',#26257,#17382,#17383);
#14179=AXIS2_PLACEMENT_3D('',#26473,#17387,#17388);
#14180=AXIS2_PLACEMENT_3D('',#26475,#17389,#17390);
#14181=AXIS2_PLACEMENT_3D('',#26689,#17393,#17394);
#14182=AXIS2_PLACEMENT_3D('',#26905,#17398,#17399);
#14183=AXIS2_PLACEMENT_3D('',#26907,#17400,#17401);
#14184=AXIS2_PLACEMENT_3D('',#27121,#17404,#17405);
#14185=AXIS2_PLACEMENT_3D('',#27337,#17409,#17410);
#14186=AXIS2_PLACEMENT_3D('',#27339,#17411,#17412);
#14187=AXIS2_PLACEMENT_3D('',#27553,#17415,#17416);
#14188=AXIS2_PLACEMENT_3D('',#27769,#17420,#17421);
#14189=AXIS2_PLACEMENT_3D('',#27771,#17422,#17423);
#14190=AXIS2_PLACEMENT_3D('',#27985,#17426,#17427);
#14191=AXIS2_PLACEMENT_3D('',#28201,#17431,#17432);
#14192=AXIS2_PLACEMENT_3D('',#28203,#17433,#17434);
#14193=AXIS2_PLACEMENT_3D('',#28417,#17437,#17438);
#14194=AXIS2_PLACEMENT_3D('',#28633,#17442,#17443);
#14195=AXIS2_PLACEMENT_3D('',#28635,#17444,#17445);
#14196=AXIS2_PLACEMENT_3D('',#28849,#17448,#17449);
#14197=AXIS2_PLACEMENT_3D('',#29065,#17453,#17454);
#14198=AXIS2_PLACEMENT_3D('',#29067,#17455,#17456);
#14199=AXIS2_PLACEMENT_3D('',#29281,#17459,#17460);
#14200=AXIS2_PLACEMENT_3D('',#29497,#17464,#17465);
#14201=AXIS2_PLACEMENT_3D('',#29499,#17466,#17467);
#14202=AXIS2_PLACEMENT_3D('',#29713,#17470,#17471);
#14203=AXIS2_PLACEMENT_3D('',#29929,#17475,#17476);
#14204=AXIS2_PLACEMENT_3D('',#29931,#17477,#17478);
#14205=AXIS2_PLACEMENT_3D('',#30145,#17481,#17482);
#14206=AXIS2_PLACEMENT_3D('',#30361,#17486,#17487);
#14207=AXIS2_PLACEMENT_3D('',#30363,#17488,#17489);
#14208=AXIS2_PLACEMENT_3D('',#30577,#17492,#17493);
#14209=AXIS2_PLACEMENT_3D('',#30793,#17497,#17498);
#14210=AXIS2_PLACEMENT_3D('',#30795,#17499,#17500);
#14211=AXIS2_PLACEMENT_3D('',#31009,#17503,#17504);
#14212=AXIS2_PLACEMENT_3D('',#31225,#17508,#17509);
#14213=AXIS2_PLACEMENT_3D('',#31227,#17510,#17511);
#14214=AXIS2_PLACEMENT_3D('',#31441,#17514,#17515);
#14215=AXIS2_PLACEMENT_3D('',#31657,#17519,#17520);
#14216=AXIS2_PLACEMENT_3D('',#31659,#17521,#17522);
#14217=AXIS2_PLACEMENT_3D('',#31873,#17525,#17526);
#14218=AXIS2_PLACEMENT_3D('',#32089,#17530,#17531);
#14219=AXIS2_PLACEMENT_3D('',#32091,#17532,#17533);
#14220=AXIS2_PLACEMENT_3D('',#32305,#17536,#17537);
#14221=AXIS2_PLACEMENT_3D('',#32521,#17541,#17542);
#14222=AXIS2_PLACEMENT_3D('',#32523,#17543,#17544);
#14223=AXIS2_PLACEMENT_3D('',#32737,#17547,#17548);
#14224=AXIS2_PLACEMENT_3D('',#32953,#17552,#17553);
#14225=AXIS2_PLACEMENT_3D('',#32954,#17554,#17555);
#14226=AXIS2_PLACEMENT_3D('',#32955,#17556,#17557);
#14227=AXIS2_PLACEMENT_3D('',#32956,#17558,#17559);
#14228=AXIS2_PLACEMENT_3D('',#32957,#17560,#17561);
#14229=AXIS2_PLACEMENT_3D('',#32959,#17562,#17563);
#14230=AXIS2_PLACEMENT_3D('',#32962,#17565,#17566);
#14231=AXIS2_PLACEMENT_3D('',#32963,#17567,#17568);
#14232=AXIS2_PLACEMENT_3D('',#32965,#17569,#17570);
#14233=AXIS2_PLACEMENT_3D('',#32968,#17572,#17573);
#14234=AXIS2_PLACEMENT_3D('',#32969,#17574,#17575);
#14235=AXIS2_PLACEMENT_3D('',#32970,#17576,#17577);
#14236=AXIS2_PLACEMENT_3D('',#32971,#17578,#17579);
#14237=AXIS2_PLACEMENT_3D('',#32972,#17580,#17581);
#14238=AXIS2_PLACEMENT_3D('',#32974,#17582,#17583);
#14239=AXIS2_PLACEMENT_3D('',#32975,#17584,#17585);
#14240=AXIS2_PLACEMENT_3D('',#32977,#17586,#17587);
#14241=AXIS2_PLACEMENT_3D('',#32979,#17589,#17590);
#14242=AXIS2_PLACEMENT_3D('',#32981,#17591,#17592);
#14243=AXIS2_PLACEMENT_3D('',#32983,#17594,#17595);
#14244=AXIS2_PLACEMENT_3D('',#32985,#17596,#17597);
#14245=AXIS2_PLACEMENT_3D('',#32987,#17599,#17600);
#14246=AXIS2_PLACEMENT_3D('',#32989,#17601,#17602);
#14247=AXIS2_PLACEMENT_3D('',#32990,#17603,#17604);
#14248=AXIS2_PLACEMENT_3D('',#32992,#17605,#17606);
#14249=AXIS2_PLACEMENT_3D('',#32994,#17608,#17609);
#14250=AXIS2_PLACEMENT_3D('',#32996,#17610,#17611);
#14251=AXIS2_PLACEMENT_3D('',#32998,#17613,#17614);
#14252=AXIS2_PLACEMENT_3D('',#33000,#17615,#17616);
#14253=AXIS2_PLACEMENT_3D('',#33002,#17618,#17619);
#14254=AXIS2_PLACEMENT_3D('',#33003,#17620,#17621);
#14255=AXIS2_PLACEMENT_3D('',#33012,#17626,#17627);
#14256=AXIS2_PLACEMENT_3D('',#33018,#17631,#17632);
#14257=AXIS2_PLACEMENT_3D('',#33024,#17636,#17637);
#14258=AXIS2_PLACEMENT_3D('',#33030,#17641,#17642);
#14259=AXIS2_PLACEMENT_3D('',#33036,#17646,#17647);
#14260=AXIS2_PLACEMENT_3D('',#33039,#17650,#17651);
#14261=AXIS2_PLACEMENT_3D('',#33040,#17652,#17653);
#14262=AXIS2_PLACEMENT_3D('',#33041,#17654,#17655);
#14263=AXIS2_PLACEMENT_3D('',#33042,#17656,#17657);
#14264=AXIS2_PLACEMENT_3D('',#33044,#17658,#17659);
#14265=AXIS2_PLACEMENT_3D('',#33045,#17660,#17661);
#14266=AXIS2_PLACEMENT_3D('',#33047,#17662,#17663);
#14267=AXIS2_PLACEMENT_3D('',#33049,#17665,#17666);
#14268=AXIS2_PLACEMENT_3D('',#33051,#17667,#17668);
#14269=AXIS2_PLACEMENT_3D('',#33053,#17670,#17671);
#14270=AXIS2_PLACEMENT_3D('',#33055,#17672,#17673);
#14271=AXIS2_PLACEMENT_3D('',#33057,#17675,#17676);
#14272=AXIS2_PLACEMENT_3D('',#33059,#17677,#17678);
#14273=AXIS2_PLACEMENT_3D('',#33060,#17679,#17680);
#14274=AXIS2_PLACEMENT_3D('',#33062,#17681,#17682);
#14275=AXIS2_PLACEMENT_3D('',#33064,#17684,#17685);
#14276=AXIS2_PLACEMENT_3D('',#33066,#17686,#17687);
#14277=AXIS2_PLACEMENT_3D('',#33068,#17689,#17690);
#14278=AXIS2_PLACEMENT_3D('',#33070,#17691,#17692);
#14279=AXIS2_PLACEMENT_3D('',#33072,#17694,#17695);
#14280=AXIS2_PLACEMENT_3D('',#33073,#17696,#17697);
#14281=AXIS2_PLACEMENT_3D('',#33082,#17702,#17703);
#14282=AXIS2_PLACEMENT_3D('',#33088,#17707,#17708);
#14283=AXIS2_PLACEMENT_3D('',#33094,#17712,#17713);
#14284=AXIS2_PLACEMENT_3D('',#33100,#17717,#17718);
#14285=AXIS2_PLACEMENT_3D('',#33106,#17722,#17723);
#14286=AXIS2_PLACEMENT_3D('',#33109,#17726,#17727);
#14287=AXIS2_PLACEMENT_3D('',#33110,#17728,#17729);
#14288=AXIS2_PLACEMENT_3D('',#33111,#17730,#17731);
#14289=AXIS2_PLACEMENT_3D('',#33112,#17732,#17733);
#14290=AXIS2_PLACEMENT_3D('',#33113,#17734,#17735);
#14291=AXIS2_PLACEMENT_3D('',#33114,#17736,#17737);
#14292=AXIS2_PLACEMENT_3D('',#33115,#17738,#17739);
#14293=AXIS2_PLACEMENT_3D('',#33116,#17740,#17741);
#14294=AXIS2_PLACEMENT_3D('',#33117,#17742,#17743);
#14295=AXIS2_PLACEMENT_3D('',#33118,#17744,#17745);
#14296=AXIS2_PLACEMENT_3D('',#33119,#17746,#17747);
#14297=AXIS2_PLACEMENT_3D('',#33120,#17748,#17749);
#14298=AXIS2_PLACEMENT_3D('',#33121,#17750,#17751);
#14299=AXIS2_PLACEMENT_3D('',#33122,#17752,#17753);
#14300=AXIS2_PLACEMENT_3D('',#33123,#17754,#17755);
#14301=AXIS2_PLACEMENT_3D('',#33124,#17756,#17757);
#14302=AXIS2_PLACEMENT_3D('',#33125,#17758,#17759);
#14303=AXIS2_PLACEMENT_3D('',#33126,#17760,#17761);
#14304=AXIS2_PLACEMENT_3D('',#33127,#17762,#17763);
#14305=AXIS2_PLACEMENT_3D('',#33128,#17764,#17765);
#14306=AXIS2_PLACEMENT_3D('',#33129,#17766,#17767);
#14307=AXIS2_PLACEMENT_3D('',#33130,#17768,#17769);
#14308=AXIS2_PLACEMENT_3D('',#33131,#17770,#17771);
#14309=AXIS2_PLACEMENT_3D('',#33132,#17772,#17773);
#14310=AXIS2_PLACEMENT_3D('',#33133,#17774,#17775);
#14311=AXIS2_PLACEMENT_3D('',#33134,#17776,#17777);
#14312=AXIS2_PLACEMENT_3D('',#33135,#17778,#17779);
#14313=AXIS2_PLACEMENT_3D('',#33136,#17780,#17781);
#14314=AXIS2_PLACEMENT_3D('',#33137,#17782,#17783);
#14315=AXIS2_PLACEMENT_3D('',#33138,#17784,#17785);
#14316=AXIS2_PLACEMENT_3D('',#33139,#17786,#17787);
#14317=AXIS2_PLACEMENT_3D('',#33140,#17788,#17789);
#14318=AXIS2_PLACEMENT_3D('',#33141,#17790,#17791);
#14319=AXIS2_PLACEMENT_3D('',#33142,#17792,#17793);
#14320=AXIS2_PLACEMENT_3D('',#33143,#17794,#17795);
#14321=AXIS2_PLACEMENT_3D('',#33144,#17796,#17797);
#14322=AXIS2_PLACEMENT_3D('',#33145,#17798,#17799);
#14323=AXIS2_PLACEMENT_3D('',#33146,#17800,#17801);
#14324=AXIS2_PLACEMENT_3D('',#33147,#17802,#17803);
#14325=AXIS2_PLACEMENT_3D('',#33148,#17804,#17805);
#14326=AXIS2_PLACEMENT_3D('',#33149,#17806,#17807);
#14327=AXIS2_PLACEMENT_3D('',#33150,#17808,#17809);
#14328=AXIS2_PLACEMENT_3D('',#33151,#17810,#17811);
#14329=AXIS2_PLACEMENT_3D('',#33152,#17812,#17813);
#14330=AXIS2_PLACEMENT_3D('',#33153,#17814,#17815);
#14331=AXIS2_PLACEMENT_3D('',#33154,#17816,#17817);
#14332=AXIS2_PLACEMENT_3D('',#33155,#17818,#17819);
#14333=AXIS2_PLACEMENT_3D('',#33156,#17820,#17821);
#14334=AXIS2_PLACEMENT_3D('',#33157,#17822,#17823);
#14335=AXIS2_PLACEMENT_3D('',#33158,#17824,#17825);
#14336=AXIS2_PLACEMENT_3D('',#33159,#17826,#17827);
#14337=AXIS2_PLACEMENT_3D('',#33160,#17828,#17829);
#14338=AXIS2_PLACEMENT_3D('',#33161,#17830,#17831);
#14339=AXIS2_PLACEMENT_3D('',#33162,#17832,#17833);
#14340=AXIS2_PLACEMENT_3D('',#33163,#17834,#17835);
#14341=AXIS2_PLACEMENT_3D('',#33164,#17836,#17837);
#14342=AXIS2_PLACEMENT_3D('',#33165,#17838,#17839);
#14343=AXIS2_PLACEMENT_3D('',#33166,#17840,#17841);
#14344=AXIS2_PLACEMENT_3D('',#33167,#17842,#17843);
#14345=AXIS2_PLACEMENT_3D('',#33168,#17844,#17845);
#14346=AXIS2_PLACEMENT_3D('',#33169,#17846,#17847);
#14347=AXIS2_PLACEMENT_3D('',#33170,#17848,#17849);
#14348=AXIS2_PLACEMENT_3D('',#33171,#17850,#17851);
#14349=AXIS2_PLACEMENT_3D('',#33172,#17852,#17853);
#14350=AXIS2_PLACEMENT_3D('',#33173,#17854,#17855);
#14351=AXIS2_PLACEMENT_3D('',#33174,#17856,#17857);
#14352=AXIS2_PLACEMENT_3D('',#33175,#17858,#17859);
#14353=AXIS2_PLACEMENT_3D('',#33176,#17860,#17861);
#14354=AXIS2_PLACEMENT_3D('',#33177,#17862,#17863);
#14355=AXIS2_PLACEMENT_3D('',#33179,#17864,#17865);
#14356=AXIS2_PLACEMENT_3D('',#33182,#17867,#17868);
#14357=AXIS2_PLACEMENT_3D('',#33183,#17869,#17870);
#14358=AXIS2_PLACEMENT_3D('',#33185,#17871,#17872);
#14359=AXIS2_PLACEMENT_3D('',#33188,#17874,#17875);
#14360=AXIS2_PLACEMENT_3D('',#33189,#17876,#17877);
#14361=AXIS2_PLACEMENT_3D('',#33190,#17878,#17879);
#14362=AXIS2_PLACEMENT_3D('',#33191,#17880,#17881);
#14363=AXIS2_PLACEMENT_3D('',#33192,#17882,#17883);
#14364=AXIS2_PLACEMENT_3D('',#33193,#17884,#17885);
#14365=AXIS2_PLACEMENT_3D('',#33194,#17886,#17887);
#14366=AXIS2_PLACEMENT_3D('',#33195,#17888,#17889);
#14367=DIRECTION('axis',(0.,0.,1.));
#14368=DIRECTION('refdir',(1.,0.,0.));
#14369=DIRECTION('axis',(0.,0.,1.));
#14370=DIRECTION('refdir',(1.,0.,0.));
#14371=DIRECTION('axis',(0.,0.,1.));
#14372=DIRECTION('refdir',(1.,0.,0.));
#14373=DIRECTION('center_axis',(0.,0.,1.));
#14374=DIRECTION('ref_axis',(1.,0.,0.));
#14375=DIRECTION('center_axis',(0.,0.,1.));
#14376=DIRECTION('ref_axis',(1.,0.,0.));
#14377=DIRECTION('',(0.,0.,1.));
#14378=DIRECTION('center_axis',(0.,0.,-1.));
#14379=DIRECTION('ref_axis',(1.,0.,0.));
#14380=DIRECTION('center_axis',(0.,0.,1.));
#14381=DIRECTION('ref_axis',(1.,0.,0.));
#14382=DIRECTION('center_axis',(0.,0.,1.));
#14383=DIRECTION('ref_axis',(1.,0.,0.));
#14384=DIRECTION('',(0.,0.,1.));
#14385=DIRECTION('center_axis',(0.,0.,-1.));
#14386=DIRECTION('ref_axis',(1.,0.,0.));
#14387=DIRECTION('center_axis',(0.,0.,1.));
#14388=DIRECTION('ref_axis',(1.,0.,0.));
#14389=DIRECTION('center_axis',(0.,0.,1.));
#14390=DIRECTION('ref_axis',(1.,0.,0.));
#14391=DIRECTION('',(0.,0.,1.));
#14392=DIRECTION('center_axis',(0.,0.,-1.));
#14393=DIRECTION('ref_axis',(1.,0.,0.));
#14394=DIRECTION('center_axis',(0.,0.,1.));
#14395=DIRECTION('ref_axis',(1.,0.,0.));
#14396=DIRECTION('center_axis',(0.,0.,1.));
#14397=DIRECTION('ref_axis',(1.,0.,0.));
#14398=DIRECTION('',(0.,0.,1.));
#14399=DIRECTION('center_axis',(0.,0.,-1.));
#14400=DIRECTION('ref_axis',(1.,0.,0.));
#14401=DIRECTION('center_axis',(0.,0.,1.));
#14402=DIRECTION('ref_axis',(1.,0.,0.));
#14403=DIRECTION('center_axis',(0.,0.,1.));
#14404=DIRECTION('ref_axis',(1.,0.,0.));
#14405=DIRECTION('',(0.,0.,1.));
#14406=DIRECTION('center_axis',(0.,0.,-1.));
#14407=DIRECTION('ref_axis',(1.,0.,0.));
#14408=DIRECTION('center_axis',(0.,0.,1.));
#14409=DIRECTION('ref_axis',(1.,0.,0.));
#14410=DIRECTION('center_axis',(0.,0.,1.));
#14411=DIRECTION('ref_axis',(1.,0.,0.));
#14412=DIRECTION('',(0.,0.,1.));
#14413=DIRECTION('center_axis',(0.,0.,-1.));
#14414=DIRECTION('ref_axis',(1.,0.,0.));
#14415=DIRECTION('center_axis',(0.,1.,0.));
#14416=DIRECTION('ref_axis',(-1.,0.,0.));
#14417=DIRECTION('',(-1.,0.,0.));
#14418=DIRECTION('',(0.,0.,1.));
#14419=DIRECTION('',(-1.,0.,0.));
#14420=DIRECTION('',(0.,0.,1.));
#14421=DIRECTION('center_axis',(1.,0.,0.));
#14422=DIRECTION('ref_axis',(0.,1.,0.));
#14423=DIRECTION('',(0.,1.,0.));
#14424=DIRECTION('',(0.,1.,0.));
#14425=DIRECTION('',(0.,0.,1.));
#14426=DIRECTION('center_axis',(0.,-1.,0.));
#14427=DIRECTION('ref_axis',(1.,0.,0.));
#14428=DIRECTION('',(1.,0.,0.));
#14429=DIRECTION('',(1.,0.,0.));
#14430=DIRECTION('',(0.,0.,1.));
#14431=DIRECTION('center_axis',(-1.,0.,0.));
#14432=DIRECTION('ref_axis',(0.,-1.,0.));
#14433=DIRECTION('',(0.,-1.,0.));
#14434=DIRECTION('',(0.,-1.,0.));
#14435=DIRECTION('center_axis',(0.,0.,1.));
#14436=DIRECTION('ref_axis',(1.,0.,0.));
#14437=DIRECTION('center_axis',(0.,0.,1.));
#14438=DIRECTION('ref_axis',(1.,0.,0.));
#14439=DIRECTION('axis',(0.,0.,1.));
#14440=DIRECTION('refdir',(1.,0.,0.));
#14441=DIRECTION('center_axis',(0.,1.,0.));
#14442=DIRECTION('ref_axis',(-1.,0.,0.));
#14443=DIRECTION('',(-1.,0.,0.));
#14444=DIRECTION('',(0.,0.,1.));
#14445=DIRECTION('',(-1.,0.,0.));
#14446=DIRECTION('',(0.,0.,1.));
#14447=DIRECTION('center_axis',(1.,0.,0.));
#14448=DIRECTION('ref_axis',(0.,1.,0.));
#14449=DIRECTION('',(0.,1.,0.));
#14450=DIRECTION('',(0.,1.,0.));
#14451=DIRECTION('',(0.,0.,1.));
#14452=DIRECTION('center_axis',(0.,-1.,0.));
#14453=DIRECTION('ref_axis',(1.,0.,0.));
#14454=DIRECTION('',(1.,0.,0.));
#14455=DIRECTION('',(1.,0.,0.));
#14456=DIRECTION('',(0.,0.,1.));
#14457=DIRECTION('center_axis',(-1.,0.,0.));
#14458=DIRECTION('ref_axis',(0.,-1.,0.));
#14459=DIRECTION('',(0.,-1.,0.));
#14460=DIRECTION('',(0.,-1.,0.));
#14461=DIRECTION('center_axis',(0.,0.,1.));
#14462=DIRECTION('ref_axis',(1.,0.,0.));
#14463=DIRECTION('center_axis',(0.,0.,1.));
#14464=DIRECTION('ref_axis',(1.,0.,0.));
#14465=DIRECTION('axis',(0.,0.,1.));
#14466=DIRECTION('refdir',(1.,0.,0.));
#14467=DIRECTION('center_axis',(0.,1.,0.));
#14468=DIRECTION('ref_axis',(-1.,0.,0.));
#14469=DIRECTION('',(-1.,0.,0.));
#14470=DIRECTION('',(0.,0.,1.));
#14471=DIRECTION('',(-1.,0.,0.));
#14472=DIRECTION('',(0.,0.,1.));
#14473=DIRECTION('center_axis',(1.,0.,0.));
#14474=DIRECTION('ref_axis',(0.,1.,0.));
#14475=DIRECTION('',(0.,1.,0.));
#14476=DIRECTION('',(0.,1.,0.));
#14477=DIRECTION('',(0.,0.,1.));
#14478=DIRECTION('center_axis',(0.,-1.,0.));
#14479=DIRECTION('ref_axis',(1.,0.,0.));
#14480=DIRECTION('',(1.,0.,0.));
#14481=DIRECTION('',(1.,0.,0.));
#14482=DIRECTION('',(0.,0.,1.));
#14483=DIRECTION('center_axis',(-1.,0.,0.));
#14484=DIRECTION('ref_axis',(0.,-1.,0.));
#14485=DIRECTION('',(0.,-1.,0.));
#14486=DIRECTION('',(0.,-1.,0.));
#14487=DIRECTION('center_axis',(0.,0.,1.));
#14488=DIRECTION('ref_axis',(1.,0.,0.));
#14489=DIRECTION('center_axis',(0.,0.,1.));
#14490=DIRECTION('ref_axis',(1.,0.,0.));
#14491=DIRECTION('axis',(0.,0.,1.));
#14492=DIRECTION('refdir',(1.,0.,0.));
#14493=DIRECTION('center_axis',(0.,0.,1.));
#14494=DIRECTION('ref_axis',(1.,0.,0.));
#14495=DIRECTION('center_axis',(0.,0.,1.));
#14496=DIRECTION('ref_axis',(1.,0.,0.));
#14497=DIRECTION('',(0.,0.,1.));
#14498=DIRECTION('center_axis',(0.,0.,-1.));
#14499=DIRECTION('ref_axis',(1.,0.,0.));
#14500=DIRECTION('center_axis',(0.,0.,1.));
#14501=DIRECTION('ref_axis',(1.,0.,0.));
#14502=DIRECTION('center_axis',(0.,0.,1.));
#14503=DIRECTION('ref_axis',(1.,0.,0.));
#14504=DIRECTION('center_axis',(0.,0.,1.));
#14505=DIRECTION('ref_axis',(1.,0.,0.));
#14506=DIRECTION('',(0.,0.,1.));
#14507=DIRECTION('center_axis',(0.,0.,-1.));
#14508=DIRECTION('ref_axis',(1.,0.,0.));
#14509=DIRECTION('center_axis',(0.,0.,1.));
#14510=DIRECTION('ref_axis',(1.,0.,0.));
#14511=DIRECTION('center_axis',(0.,1.,0.));
#14512=DIRECTION('ref_axis',(-1.,0.,0.));
#14513=DIRECTION('',(0.,0.,1.));
#14514=DIRECTION('',(-1.,0.,0.));
#14515=DIRECTION('',(0.,0.,-1.));
#14516=DIRECTION('',(1.,0.,0.));
#14517=DIRECTION('center_axis',(0.,-1.,0.));
#14518=DIRECTION('ref_axis',(1.,0.,0.));
#14519=DIRECTION('',(0.,0.,-1.));
#14520=DIRECTION('',(-1.,0.,0.));
#14521=DIRECTION('',(0.,0.,1.));
#14522=DIRECTION('',(1.,0.,0.));
#14523=DIRECTION('center_axis',(0.,0.,1.));
#14524=DIRECTION('ref_axis',(1.,0.,0.));
#14525=DIRECTION('center_axis',(0.,0.,1.));
#14526=DIRECTION('ref_axis',(1.,0.,0.));
#14527=DIRECTION('',(-1.,0.,0.));
#14528=DIRECTION('',(0.,1.,0.));
#14529=DIRECTION('',(1.,0.,0.));
#14530=DIRECTION('center_axis',(0.,0.,1.));
#14531=DIRECTION('ref_axis',(1.,0.,0.));
#14532=DIRECTION('center_axis',(0.,0.,1.));
#14533=DIRECTION('ref_axis',(1.,0.,0.));
#14534=DIRECTION('center_axis',(0.,0.,1.));
#14535=DIRECTION('ref_axis',(1.,0.,0.));
#14536=DIRECTION('center_axis',(0.,0.,-1.));
#14537=DIRECTION('ref_axis',(1.,0.,0.));
#14538=DIRECTION('center_axis',(0.,0.,1.));
#14539=DIRECTION('ref_axis',(1.,0.,0.));
#14540=DIRECTION('',(0.,0.,1.));
#14541=DIRECTION('center_axis',(0.,0.,1.));
#14542=DIRECTION('ref_axis',(1.,0.,0.));
#14543=DIRECTION('center_axis',(0.,0.,1.));
#14544=DIRECTION('ref_axis',(1.,0.,0.));
#14545=DIRECTION('center_axis',(0.,0.,1.));
#14546=DIRECTION('ref_axis',(1.,0.,0.));
#14547=DIRECTION('',(0.,0.,1.));
#14548=DIRECTION('center_axis',(0.,0.,1.));
#14549=DIRECTION('ref_axis',(1.,0.,0.));
#14550=DIRECTION('',(1.,0.,0.));
#14551=DIRECTION('',(0.,-1.,0.));
#14552=DIRECTION('',(-1.,0.,0.));
#14553=DIRECTION('center_axis',(0.,-1.,0.));
#14554=DIRECTION('ref_axis',(1.,0.,0.));
#14555=DIRECTION('',(0.,0.,-1.));
#14556=DIRECTION('center_axis',(0.,1.,0.));
#14557=DIRECTION('ref_axis',(-1.,0.,0.));
#14558=DIRECTION('',(0.,0.,1.));
#14559=DIRECTION('center_axis',(0.,0.,1.));
#14560=DIRECTION('ref_axis',(1.,0.,0.));
#14561=DIRECTION('center_axis',(0.,0.,1.));
#14562=DIRECTION('ref_axis',(1.,0.,0.));
#14563=DIRECTION('',(0.,0.,1.));
#14564=DIRECTION('center_axis',(0.,0.,-1.));
#14565=DIRECTION('ref_axis',(1.,0.,0.));
#14566=DIRECTION('center_axis',(0.,0.,1.));
#14567=DIRECTION('ref_axis',(1.,0.,0.));
#14568=DIRECTION('center_axis',(0.,0.,1.));
#14569=DIRECTION('ref_axis',(1.,0.,0.));
#14570=DIRECTION('center_axis',(0.,0.,1.));
#14571=DIRECTION('ref_axis',(1.,0.,0.));
#14572=DIRECTION('',(0.,0.,1.));
#14573=DIRECTION('center_axis',(0.,0.,-1.));
#14574=DIRECTION('ref_axis',(1.,0.,0.));
#14575=DIRECTION('center_axis',(0.,0.,1.));
#14576=DIRECTION('ref_axis',(1.,0.,0.));
#14577=DIRECTION('center_axis',(0.,1.,0.));
#14578=DIRECTION('ref_axis',(-1.,0.,0.));
#14579=DIRECTION('',(0.,0.,1.));
#14580=DIRECTION('',(-1.,0.,0.));
#14581=DIRECTION('',(0.,0.,-1.));
#14582=DIRECTION('',(1.,0.,0.));
#14583=DIRECTION('center_axis',(0.,-1.,0.));
#14584=DIRECTION('ref_axis',(1.,0.,0.));
#14585=DIRECTION('',(0.,0.,-1.));
#14586=DIRECTION('',(-1.,0.,0.));
#14587=DIRECTION('',(0.,0.,1.));
#14588=DIRECTION('',(1.,0.,0.));
#14589=DIRECTION('center_axis',(0.,0.,1.));
#14590=DIRECTION('ref_axis',(1.,0.,0.));
#14591=DIRECTION('center_axis',(0.,0.,1.));
#14592=DIRECTION('ref_axis',(1.,0.,0.));
#14593=DIRECTION('',(-1.,0.,0.));
#14594=DIRECTION('',(0.,-1.,0.));
#14595=DIRECTION('',(-1.,0.,0.));
#14596=DIRECTION('',(0.,1.,0.));
#14597=DIRECTION('center_axis',(0.,0.,1.));
#14598=DIRECTION('ref_axis',(1.,0.,0.));
#14599=DIRECTION('center_axis',(0.,0.,1.));
#14600=DIRECTION('ref_axis',(1.,0.,0.));
#14601=DIRECTION('',(0.,1.,0.));
#14602=DIRECTION('',(1.,0.,0.));
#14603=DIRECTION('',(0.,-1.,0.));
#14604=DIRECTION('',(1.,0.,0.));
#14605=DIRECTION('center_axis',(0.,0.,1.));
#14606=DIRECTION('ref_axis',(1.,0.,0.));
#14607=DIRECTION('center_axis',(0.,0.,1.));
#14608=DIRECTION('ref_axis',(1.,0.,0.));
#14609=DIRECTION('center_axis',(0.,0.,1.));
#14610=DIRECTION('ref_axis',(1.,0.,0.));
#14611=DIRECTION('center_axis',(0.,0.,-1.));
#14612=DIRECTION('ref_axis',(1.,0.,0.));
#14613=DIRECTION('center_axis',(0.,0.,1.));
#14614=DIRECTION('ref_axis',(1.,0.,0.));
#14615=DIRECTION('',(0.,0.,1.));
#14616=DIRECTION('center_axis',(0.,0.,1.));
#14617=DIRECTION('ref_axis',(1.,0.,0.));
#14618=DIRECTION('center_axis',(0.,0.,1.));
#14619=DIRECTION('ref_axis',(1.,0.,0.));
#14620=DIRECTION('center_axis',(0.,0.,1.));
#14621=DIRECTION('ref_axis',(1.,0.,0.));
#14622=DIRECTION('',(0.,0.,1.));
#14623=DIRECTION('center_axis',(0.,0.,1.));
#14624=DIRECTION('ref_axis',(1.,0.,0.));
#14625=DIRECTION('',(1.,0.,0.));
#14626=DIRECTION('',(0.,-1.,0.));
#14627=DIRECTION('',(-1.,0.,0.));
#14628=DIRECTION('center_axis',(0.,1.,0.));
#14629=DIRECTION('ref_axis',(-1.,0.,0.));
#14630=DIRECTION('',(0.,0.,1.));
#14631=DIRECTION('center_axis',(0.,-1.,0.));
#14632=DIRECTION('ref_axis',(1.,0.,0.));
#14633=DIRECTION('',(0.,0.,-1.));
#14634=DIRECTION('center_axis',(-1.,0.,0.));
#14635=DIRECTION('ref_axis',(0.,-1.,0.));
#14636=DIRECTION('',(0.,0.,1.));
#14637=DIRECTION('',(0.,-1.,0.));
#14638=DIRECTION('',(0.,0.,1.));
#14639=DIRECTION('center_axis',(1.,0.,0.));
#14640=DIRECTION('ref_axis',(0.,0.,-1.));
#14641=DIRECTION('',(0.,0.,1.));
#14642=DIRECTION('center_axis',(1.,0.,0.));
#14643=DIRECTION('ref_axis',(0.,0.,-1.));
#14644=DIRECTION('center_axis',(1.,0.,0.));
#14645=DIRECTION('ref_axis',(0.,0.,-1.));
#14646=DIRECTION('center_axis',(1.,0.,0.));
#14647=DIRECTION('ref_axis',(0.,0.,-1.));
#14648=DIRECTION('',(1.,0.,0.));
#14649=DIRECTION('center_axis',(1.,0.,0.));
#14650=DIRECTION('ref_axis',(0.,0.,-1.));
#14651=DIRECTION('',(0.,0.,-1.));
#14652=DIRECTION('center_axis',(0.,0.,1.));
#14653=DIRECTION('ref_axis',(1.,0.,0.));
#14654=DIRECTION('',(0.,1.,0.));
#14655=DIRECTION('center_axis',(0.,0.,1.));
#14656=DIRECTION('ref_axis',(1.,0.,0.));
#14657=DIRECTION('center_axis',(0.,0.,1.));
#14658=DIRECTION('ref_axis',(1.,0.,0.));
#14659=DIRECTION('center_axis',(0.,0.,-1.));
#14660=DIRECTION('ref_axis',(1.,0.,0.));
#14661=DIRECTION('',(0.,0.,-1.));
#14662=DIRECTION('center_axis',(0.,0.,-1.));
#14663=DIRECTION('ref_axis',(1.,0.,0.));
#14664=DIRECTION('center_axis',(0.,0.,1.));
#14665=DIRECTION('ref_axis',(1.,0.,0.));
#14666=DIRECTION('',(0.,0.,-1.));
#14667=DIRECTION('center_axis',(0.,0.,1.));
#14668=DIRECTION('ref_axis',(1.,0.,0.));
#14669=DIRECTION('center_axis',(0.,0.,1.));
#14670=DIRECTION('ref_axis',(1.,0.,0.));
#14671=DIRECTION('center_axis',(0.,1.,0.));
#14672=DIRECTION('ref_axis',(-1.,0.,0.));
#14673=DIRECTION('',(-1.,0.,0.));
#14674=DIRECTION('',(0.,0.,1.));
#14675=DIRECTION('center_axis',(1.,0.,0.));
#14676=DIRECTION('ref_axis',(0.,1.,0.));
#14677=DIRECTION('',(0.,1.,0.));
#14678=DIRECTION('',(0.,0.,1.));
#14679=DIRECTION('center_axis',(0.,-1.,0.));
#14680=DIRECTION('ref_axis',(1.,0.,0.));
#14681=DIRECTION('',(1.,0.,0.));
#14682=DIRECTION('center_axis',(0.,0.,1.));
#14683=DIRECTION('ref_axis',(1.,0.,0.));
#14684=DIRECTION('center_axis',(0.,0.,1.));
#14685=DIRECTION('ref_axis',(1.,0.,0.));
#14686=DIRECTION('axis',(0.,0.,1.));
#14687=DIRECTION('refdir',(1.,0.,0.));
#14688=DIRECTION('center_axis',(0.,0.,1.));
#14689=DIRECTION('ref_axis',(1.,0.,0.));
#14690=DIRECTION('',(0.,0.,-1.));
#14691=DIRECTION('center_axis',(0.,0.,1.));
#14692=DIRECTION('ref_axis',(1.,0.,0.));
#14693=DIRECTION('',(0.,0.,1.));
#14694=DIRECTION('center_axis',(0.,0.,1.));
#14695=DIRECTION('ref_axis',(1.,0.,0.));
#14696=DIRECTION('center_axis',(0.,0.,1.));
#14697=DIRECTION('ref_axis',(1.,0.,0.));
#14698=DIRECTION('center_axis',(0.,0.,1.));
#14699=DIRECTION('ref_axis',(1.,0.,0.));
#14700=DIRECTION('center_axis',(0.,0.,1.));
#14701=DIRECTION('ref_axis',(1.,0.,0.));
#14702=DIRECTION('',(0.,0.,-1.));
#14703=DIRECTION('center_axis',(0.,0.,1.));
#14704=DIRECTION('ref_axis',(1.,0.,0.));
#14705=DIRECTION('',(0.,0.,1.));
#14706=DIRECTION('center_axis',(0.,0.,1.));
#14707=DIRECTION('ref_axis',(1.,0.,0.));
#14708=DIRECTION('center_axis',(0.,0.,1.));
#14709=DIRECTION('ref_axis',(1.,0.,0.));
#14710=DIRECTION('center_axis',(0.,0.,1.));
#14711=DIRECTION('ref_axis',(1.,0.,0.));
#14712=DIRECTION('center_axis',(0.,0.,1.));
#14713=DIRECTION('ref_axis',(1.,0.,0.));
#14714=DIRECTION('center_axis',(0.,0.,1.));
#14715=DIRECTION('ref_axis',(1.,0.,0.));
#14716=DIRECTION('center_axis',(0.,0.,-1.));
#14717=DIRECTION('ref_axis',(1.,0.,0.));
#14718=DIRECTION('center_axis',(0.,0.,-1.));
#14719=DIRECTION('ref_axis',(1.,0.,0.));
#14720=DIRECTION('center_axis',(0.,0.,-1.));
#14721=DIRECTION('ref_axis',(1.,0.,0.));
#14722=DIRECTION('center_axis',(0.,0.,1.));
#14723=DIRECTION('ref_axis',(1.,0.,0.));
#14724=DIRECTION('center_axis',(0.,0.,1.));
#14725=DIRECTION('ref_axis',(1.,0.,0.));
#14726=DIRECTION('center_axis',(1.,0.,0.));
#14727=DIRECTION('ref_axis',(0.,0.,-1.));
#14728=DIRECTION('',(0.,0.,1.));
#14729=DIRECTION('center_axis',(1.,0.,0.));
#14730=DIRECTION('ref_axis',(0.,0.,-1.));
#14731=DIRECTION('center_axis',(1.,0.,0.));
#14732=DIRECTION('ref_axis',(0.,0.,-1.));
#14733=DIRECTION('center_axis',(1.,0.,0.));
#14734=DIRECTION('ref_axis',(0.,0.,-1.));
#14735=DIRECTION('',(1.,0.,0.));
#14736=DIRECTION('center_axis',(1.,0.,0.));
#14737=DIRECTION('ref_axis',(0.,0.,-1.));
#14738=DIRECTION('',(0.,0.,-1.));
#14739=DIRECTION('center_axis',(0.,0.,1.));
#14740=DIRECTION('ref_axis',(1.,0.,0.));
#14741=DIRECTION('center_axis',(0.,0.,1.));
#14742=DIRECTION('ref_axis',(1.,0.,0.));
#14743=DIRECTION('',(0.,0.,1.));
#14744=DIRECTION('center_axis',(0.,0.,1.));
#14745=DIRECTION('ref_axis',(1.,0.,0.));
#14746=DIRECTION('center_axis',(0.,0.,1.));
#14747=DIRECTION('ref_axis',(1.,0.,0.));
#14748=DIRECTION('',(0.,0.,1.));
#14749=DIRECTION('center_axis',(0.,0.,1.));
#14750=DIRECTION('ref_axis',(1.,0.,0.));
#14751=DIRECTION('center_axis',(0.,0.,1.));
#14752=DIRECTION('ref_axis',(1.,0.,0.));
#14753=DIRECTION('',(0.,0.,-1.));
#14754=DIRECTION('center_axis',(0.,0.,1.));
#14755=DIRECTION('ref_axis',(1.,0.,0.));
#14756=DIRECTION('center_axis',(0.,0.,-1.));
#14757=DIRECTION('ref_axis',(1.,0.,0.));
#14758=DIRECTION('center_axis',(0.,0.,1.));
#14759=DIRECTION('ref_axis',(1.,0.,0.));
#14760=DIRECTION('',(0.,0.,-1.));
#14761=DIRECTION('center_axis',(0.,0.,-1.));
#14762=DIRECTION('ref_axis',(1.,0.,0.));
#14763=DIRECTION('center_axis',(0.,0.,1.));
#14764=DIRECTION('ref_axis',(1.,0.,0.));
#14765=DIRECTION('',(0.,0.,-1.));
#14766=DIRECTION('center_axis',(0.,0.,1.));
#14767=DIRECTION('ref_axis',(1.,0.,0.));
#14768=DIRECTION('center_axis',(0.,0.,1.));
#14769=DIRECTION('ref_axis',(1.,0.,0.));
#14770=DIRECTION('axis',(0.,0.,1.));
#14771=DIRECTION('refdir',(1.,0.,0.));
#14772=DIRECTION('center_axis',(1.,0.,0.));
#14773=DIRECTION('ref_axis',(0.,1.,0.));
#14774=DIRECTION('',(0.,1.,0.));
#14775=DIRECTION('',(0.,0.,1.));
#14776=DIRECTION('',(0.,-1.,0.));
#14777=DIRECTION('',(0.,0.,1.));
#14778=DIRECTION('center_axis',(1.,0.,0.));
#14779=DIRECTION('ref_axis',(0.,1.,0.));
#14780=DIRECTION('',(0.,-1.,0.));
#14781=DIRECTION('',(0.,0.,1.));
#14782=DIRECTION('',(0.,1.,0.));
#14783=DIRECTION('',(0.,0.,-1.));
#14784=DIRECTION('center_axis',(0.,1.,0.));
#14785=DIRECTION('ref_axis',(-1.,0.,0.));
#14786=DIRECTION('',(1.,0.,0.));
#14787=DIRECTION('',(0.,0.,1.));
#14788=DIRECTION('',(-1.,0.,0.));
#14789=DIRECTION('',(0.,0.,1.));
#14790=DIRECTION('',(-1.,0.,0.));
#14791=DIRECTION('center_axis',(0.,-1.,0.));
#14792=DIRECTION('ref_axis',(1.,0.,0.));
#14793=DIRECTION('',(1.,0.,0.));
#14794=DIRECTION('',(0.,0.,-1.));
#14795=DIRECTION('',(1.,0.,0.));
#14796=DIRECTION('',(0.,0.,-1.));
#14797=DIRECTION('',(-1.,0.,0.));
#14798=DIRECTION('center_axis',(0.,0.,1.));
#14799=DIRECTION('ref_axis',(1.,0.,0.));
#14800=DIRECTION('center_axis',(0.,0.,1.));
#14801=DIRECTION('ref_axis',(1.,0.,0.));
#14802=DIRECTION('center_axis',(0.,0.,-1.));
#14803=DIRECTION('ref_axis',(1.,0.,0.));
#14804=DIRECTION('center_axis',(0.,0.,1.));
#14805=DIRECTION('ref_axis',(1.,0.,0.));
#14806=DIRECTION('center_axis',(0.,0.,-1.));
#14807=DIRECTION('ref_axis',(1.,0.,0.));
#14808=DIRECTION('center_axis',(0.,0.,1.));
#14809=DIRECTION('ref_axis',(1.,0.,0.));
#14810=DIRECTION('center_axis',(0.,0.,1.));
#14811=DIRECTION('ref_axis',(1.,0.,0.));
#14812=DIRECTION('center_axis',(0.,0.,1.));
#14813=DIRECTION('ref_axis',(1.,0.,0.));
#14814=DIRECTION('center_axis',(0.,0.,1.));
#14815=DIRECTION('ref_axis',(1.,0.,0.));
#14816=DIRECTION('center_axis',(0.,0.,1.));
#14817=DIRECTION('ref_axis',(1.,0.,0.));
#14818=DIRECTION('center_axis',(0.,0.,1.));
#14819=DIRECTION('ref_axis',(1.,0.,0.));
#14820=DIRECTION('center_axis',(0.,0.,1.));
#14821=DIRECTION('ref_axis',(1.,0.,0.));
#14822=DIRECTION('axis',(0.,0.,1.));
#14823=DIRECTION('refdir',(1.,0.,0.));
#14824=DIRECTION('center_axis',(0.,0.,1.));
#14825=DIRECTION('ref_axis',(1.,0.,0.));
#14826=DIRECTION('center_axis',(0.,0.,1.));
#14827=DIRECTION('ref_axis',(1.,0.,0.));
#14828=DIRECTION('',(0.,0.,1.));
#14829=DIRECTION('center_axis',(0.,0.,-1.));
#14830=DIRECTION('ref_axis',(1.,0.,0.));
#14831=DIRECTION('center_axis',(0.,0.,1.));
#14832=DIRECTION('ref_axis',(1.,0.,0.));
#14833=DIRECTION('center_axis',(0.,0.,1.));
#14834=DIRECTION('ref_axis',(1.,0.,0.));
#14835=DIRECTION('',(0.,0.,1.));
#14836=DIRECTION('center_axis',(0.,0.,-1.));
#14837=DIRECTION('ref_axis',(1.,0.,0.));
#14838=DIRECTION('center_axis',(0.,1.,0.));
#14839=DIRECTION('ref_axis',(-1.,0.,0.));
#14840=DIRECTION('',(-1.,0.,0.));
#14841=DIRECTION('',(0.,0.,1.));
#14842=DIRECTION('',(1.,0.,0.));
#14843=DIRECTION('',(0.,0.,1.));
#14844=DIRECTION('center_axis',(0.,-1.,0.));
#14845=DIRECTION('ref_axis',(1.,0.,0.));
#14846=DIRECTION('',(-1.,0.,0.));
#14847=DIRECTION('',(0.,0.,1.));
#14848=DIRECTION('',(1.,0.,0.));
#14849=DIRECTION('',(0.,0.,-1.));
#14850=DIRECTION('center_axis',(1.,0.,0.));
#14851=DIRECTION('ref_axis',(0.,1.,0.));
#14852=DIRECTION('',(0.,-1.,0.));
#14853=DIRECTION('',(0.,0.,1.));
#14854=DIRECTION('',(0.,1.,0.));
#14855=DIRECTION('center_axis',(1.,0.,0.));
#14856=DIRECTION('ref_axis',(0.,1.,0.));
#14857=DIRECTION('',(0.,1.,0.));
#14858=DIRECTION('',(0.,0.,-1.));
#14859=DIRECTION('',(0.,-1.,0.));
#14860=DIRECTION('center_axis',(-1.,0.,0.));
#14861=DIRECTION('ref_axis',(0.,-1.,0.));
#14862=DIRECTION('',(0.,-1.,0.));
#14863=DIRECTION('',(0.,0.,1.));
#14864=DIRECTION('',(0.,-1.,0.));
#14865=DIRECTION('center_axis',(-1.,0.,0.));
#14866=DIRECTION('ref_axis',(0.,-1.,0.));
#14867=DIRECTION('',(0.,-1.,0.));
#14868=DIRECTION('',(0.,0.,1.));
#14869=DIRECTION('',(0.,-1.,0.));
#14870=DIRECTION('center_axis',(0.,0.,1.));
#14871=DIRECTION('ref_axis',(1.,0.,0.));
#14872=DIRECTION('center_axis',(0.,0.,-1.));
#14873=DIRECTION('ref_axis',(1.,0.,0.));
#14874=DIRECTION('',(1.,0.,0.));
#14875=DIRECTION('',(0.,1.,0.));
#14876=DIRECTION('',(-1.,0.,0.));
#14877=DIRECTION('center_axis',(0.,0.,1.));
#14878=DIRECTION('ref_axis',(1.,0.,0.));
#14879=DIRECTION('center_axis',(0.,0.,1.));
#14880=DIRECTION('ref_axis',(1.,0.,0.));
#14881=DIRECTION('center_axis',(0.,1.,0.));
#14882=DIRECTION('ref_axis',(-1.,0.,0.));
#14883=DIRECTION('',(-1.,0.,0.));
#14884=DIRECTION('',(0.,0.,1.));
#14885=DIRECTION('center_axis',(1.,0.,0.));
#14886=DIRECTION('ref_axis',(0.,1.,0.));
#14887=DIRECTION('',(0.,1.,0.));
#14888=DIRECTION('',(0.,0.,1.));
#14889=DIRECTION('center_axis',(0.,-1.,0.));
#14890=DIRECTION('ref_axis',(1.,0.,0.));
#14891=DIRECTION('',(1.,0.,0.));
#14892=DIRECTION('center_axis',(0.,0.,1.));
#14893=DIRECTION('ref_axis',(1.,0.,0.));
#14894=DIRECTION('axis',(0.,0.,1.));
#14895=DIRECTION('refdir',(1.,0.,0.));
#14896=DIRECTION('center_axis',(1.,0.,0.));
#14897=DIRECTION('ref_axis',(0.,1.,0.));
#14898=DIRECTION('',(0.,1.,0.));
#14899=DIRECTION('',(0.,0.,1.));
#14900=DIRECTION('',(0.,-1.,0.));
#14901=DIRECTION('',(0.,0.,1.));
#14902=DIRECTION('center_axis',(1.,0.,0.));
#14903=DIRECTION('ref_axis',(0.,1.,0.));
#14904=DIRECTION('',(0.,-1.,0.));
#14905=DIRECTION('',(0.,0.,1.));
#14906=DIRECTION('',(0.,1.,0.));
#14907=DIRECTION('',(0.,0.,-1.));
#14908=DIRECTION('center_axis',(0.,1.,0.));
#14909=DIRECTION('ref_axis',(-1.,0.,0.));
#14910=DIRECTION('',(1.,0.,0.));
#14911=DIRECTION('',(0.,0.,1.));
#14912=DIRECTION('',(-1.,0.,0.));
#14913=DIRECTION('',(0.,0.,1.));
#14914=DIRECTION('',(-1.,0.,0.));
#14915=DIRECTION('center_axis',(0.,-1.,0.));
#14916=DIRECTION('ref_axis',(1.,0.,0.));
#14917=DIRECTION('',(1.,0.,0.));
#14918=DIRECTION('',(0.,0.,-1.));
#14919=DIRECTION('',(1.,0.,0.));
#14920=DIRECTION('',(0.,0.,-1.));
#14921=DIRECTION('',(-1.,0.,0.));
#14922=DIRECTION('center_axis',(0.,0.,1.));
#14923=DIRECTION('ref_axis',(1.,0.,0.));
#14924=DIRECTION('center_axis',(0.,0.,1.));
#14925=DIRECTION('ref_axis',(1.,0.,0.));
#14926=DIRECTION('center_axis',(0.,0.,-1.));
#14927=DIRECTION('ref_axis',(1.,0.,0.));
#14928=DIRECTION('center_axis',(0.,0.,1.));
#14929=DIRECTION('ref_axis',(1.,0.,0.));
#14930=DIRECTION('center_axis',(0.,0.,-1.));
#14931=DIRECTION('ref_axis',(1.,0.,0.));
#14932=DIRECTION('center_axis',(0.,0.,1.));
#14933=DIRECTION('ref_axis',(1.,0.,0.));
#14934=DIRECTION('center_axis',(0.,0.,1.));
#14935=DIRECTION('ref_axis',(1.,0.,0.));
#14936=DIRECTION('center_axis',(0.,0.,1.));
#14937=DIRECTION('ref_axis',(1.,0.,0.));
#14938=DIRECTION('center_axis',(0.,0.,1.));
#14939=DIRECTION('ref_axis',(1.,0.,0.));
#14940=DIRECTION('center_axis',(0.,0.,1.));
#14941=DIRECTION('ref_axis',(1.,0.,0.));
#14942=DIRECTION('center_axis',(0.,0.,1.));
#14943=DIRECTION('ref_axis',(1.,0.,0.));
#14944=DIRECTION('center_axis',(0.,0.,1.));
#14945=DIRECTION('ref_axis',(1.,0.,0.));
#14946=DIRECTION('axis',(0.,0.,1.));
#14947=DIRECTION('refdir',(1.,0.,0.));
#14948=DIRECTION('center_axis',(0.,0.,1.));
#14949=DIRECTION('ref_axis',(1.,0.,0.));
#14950=DIRECTION('center_axis',(0.,0.,1.));
#14951=DIRECTION('ref_axis',(1.,0.,0.));
#14952=DIRECTION('',(0.,0.,1.));
#14953=DIRECTION('center_axis',(0.,0.,-1.));
#14954=DIRECTION('ref_axis',(1.,0.,0.));
#14955=DIRECTION('center_axis',(0.,0.,1.));
#14956=DIRECTION('ref_axis',(1.,0.,0.));
#14957=DIRECTION('center_axis',(0.,0.,1.));
#14958=DIRECTION('ref_axis',(1.,0.,0.));
#14959=DIRECTION('',(0.,0.,1.));
#14960=DIRECTION('center_axis',(0.,0.,-1.));
#14961=DIRECTION('ref_axis',(1.,0.,0.));
#14962=DIRECTION('center_axis',(0.,1.,0.));
#14963=DIRECTION('ref_axis',(-1.,0.,0.));
#14964=DIRECTION('',(-1.,0.,0.));
#14965=DIRECTION('',(0.,0.,1.));
#14966=DIRECTION('',(1.,0.,0.));
#14967=DIRECTION('',(0.,0.,1.));
#14968=DIRECTION('center_axis',(0.,-1.,0.));
#14969=DIRECTION('ref_axis',(1.,0.,0.));
#14970=DIRECTION('',(-1.,0.,0.));
#14971=DIRECTION('',(0.,0.,1.));
#14972=DIRECTION('',(1.,0.,0.));
#14973=DIRECTION('',(0.,0.,-1.));
#14974=DIRECTION('center_axis',(1.,0.,0.));
#14975=DIRECTION('ref_axis',(0.,1.,0.));
#14976=DIRECTION('',(0.,-1.,0.));
#14977=DIRECTION('',(0.,0.,1.));
#14978=DIRECTION('',(0.,1.,0.));
#14979=DIRECTION('center_axis',(1.,0.,0.));
#14980=DIRECTION('ref_axis',(0.,1.,0.));
#14981=DIRECTION('',(0.,1.,0.));
#14982=DIRECTION('',(0.,0.,-1.));
#14983=DIRECTION('',(0.,-1.,0.));
#14984=DIRECTION('center_axis',(-1.,0.,0.));
#14985=DIRECTION('ref_axis',(0.,-1.,0.));
#14986=DIRECTION('',(0.,-1.,0.));
#14987=DIRECTION('',(0.,0.,1.));
#14988=DIRECTION('',(0.,-1.,0.));
#14989=DIRECTION('center_axis',(-1.,0.,0.));
#14990=DIRECTION('ref_axis',(0.,-1.,0.));
#14991=DIRECTION('',(0.,-1.,0.));
#14992=DIRECTION('',(0.,0.,1.));
#14993=DIRECTION('',(0.,-1.,0.));
#14994=DIRECTION('center_axis',(0.,0.,1.));
#14995=DIRECTION('ref_axis',(1.,0.,0.));
#14996=DIRECTION('center_axis',(0.,0.,-1.));
#14997=DIRECTION('ref_axis',(1.,0.,0.));
#14998=DIRECTION('',(1.,0.,0.));
#14999=DIRECTION('',(0.,1.,0.));
#15000=DIRECTION('',(-1.,0.,0.));
#15001=DIRECTION('center_axis',(0.,0.,1.));
#15002=DIRECTION('ref_axis',(1.,0.,0.));
#15003=DIRECTION('center_axis',(0.,0.,1.));
#15004=DIRECTION('ref_axis',(1.,0.,0.));
#15005=DIRECTION('center_axis',(0.,1.,0.));
#15006=DIRECTION('ref_axis',(-1.,0.,0.));
#15007=DIRECTION('',(-1.,0.,0.));
#15008=DIRECTION('',(0.,0.,1.));
#15009=DIRECTION('center_axis',(1.,0.,0.));
#15010=DIRECTION('ref_axis',(0.,1.,0.));
#15011=DIRECTION('',(0.,1.,0.));
#15012=DIRECTION('',(0.,0.,1.));
#15013=DIRECTION('center_axis',(0.,-1.,0.));
#15014=DIRECTION('ref_axis',(1.,0.,0.));
#15015=DIRECTION('',(1.,0.,0.));
#15016=DIRECTION('center_axis',(0.,0.,1.));
#15017=DIRECTION('ref_axis',(1.,0.,0.));
#15018=DIRECTION('axis',(0.,0.,1.));
#15019=DIRECTION('refdir',(1.,0.,0.));
#15020=DIRECTION('center_axis',(0.,-1.,0.));
#15021=DIRECTION('ref_axis',(1.,0.,0.));
#15022=DIRECTION('',(-1.,0.,0.));
#15023=DIRECTION('',(0.,0.,1.));
#15024=DIRECTION('',(1.,0.,0.));
#15025=DIRECTION('',(0.,0.,-1.));
#15026=DIRECTION('center_axis',(1.,0.,0.));
#15027=DIRECTION('ref_axis',(0.,1.,0.));
#15028=DIRECTION('',(0.,1.,0.));
#15029=DIRECTION('',(0.,0.,1.));
#15030=DIRECTION('',(0.,-1.,0.));
#15031=DIRECTION('center_axis',(0.,0.,1.));
#15032=DIRECTION('ref_axis',(1.,0.,0.));
#15033=DIRECTION('',(0.,1.,0.));
#15034=DIRECTION('',(-1.,0.,0.));
#15035=DIRECTION('center_axis',(0.,0.,1.));
#15036=DIRECTION('ref_axis',(1.,0.,0.));
#15037=DIRECTION('center_axis',(0.,0.,1.));
#15038=DIRECTION('ref_axis',(1.,0.,0.));
#15039=DIRECTION('center_axis',(0.,1.,0.));
#15040=DIRECTION('ref_axis',(-1.,0.,0.));
#15041=DIRECTION('',(1.,0.,0.));
#15042=DIRECTION('',(0.,0.,-1.));
#15043=DIRECTION('center_axis',(1.,0.,0.));
#15044=DIRECTION('ref_axis',(0.,1.,0.));
#15045=DIRECTION('',(0.,1.,0.));
#15046=DIRECTION('center_axis',(0.,0.,1.));
#15047=DIRECTION('ref_axis',(1.,0.,0.));
#15048=DIRECTION('center_axis',(0.,0.,-1.));
#15049=DIRECTION('ref_axis',(1.,0.,0.));
#15050=DIRECTION('center_axis',(0.,0.,-1.));
#15051=DIRECTION('ref_axis',(1.,0.,0.));
#15052=DIRECTION('center_axis',(1.,0.,0.));
#15053=DIRECTION('ref_axis',(0.,0.,-1.));
#15054=DIRECTION('',(0.,0.,1.));
#15055=DIRECTION('center_axis',(1.,0.,0.));
#15056=DIRECTION('ref_axis',(0.,0.,-1.));
#15057=DIRECTION('center_axis',(1.,0.,0.));
#15058=DIRECTION('ref_axis',(0.,0.,-1.));
#15059=DIRECTION('center_axis',(1.,0.,0.));
#15060=DIRECTION('ref_axis',(0.,0.,-1.));
#15061=DIRECTION('',(1.,0.,0.));
#15062=DIRECTION('center_axis',(1.,0.,0.));
#15063=DIRECTION('ref_axis',(0.,0.,-1.));
#15064=DIRECTION('',(0.,0.,-1.));
#15065=DIRECTION('center_axis',(0.,0.,1.));
#15066=DIRECTION('ref_axis',(1.,0.,0.));
#15067=DIRECTION('',(0.,0.,1.));
#15068=DIRECTION('center_axis',(0.,0.,1.));
#15069=DIRECTION('ref_axis',(1.,0.,0.));
#15070=DIRECTION('center_axis',(0.,0.,1.));
#15071=DIRECTION('ref_axis',(1.,0.,0.));
#15072=DIRECTION('',(0.,0.,1.));
#15073=DIRECTION('center_axis',(0.,0.,1.));
#15074=DIRECTION('ref_axis',(1.,0.,0.));
#15075=DIRECTION('',(0.,0.,-1.));
#15076=DIRECTION('center_axis',(0.,0.,1.));
#15077=DIRECTION('ref_axis',(1.,0.,0.));
#15078=DIRECTION('center_axis',(0.,0.,1.));
#15079=DIRECTION('ref_axis',(1.,0.,0.));
#15080=DIRECTION('axis',(0.,0.,1.));
#15081=DIRECTION('refdir',(1.,0.,0.));
#15082=DIRECTION('center_axis',(0.,1.,0.));
#15083=DIRECTION('ref_axis',(1.,0.,0.));
#15084=DIRECTION('center_axis',(0.,1.,0.));
#15085=DIRECTION('ref_axis',(1.,0.,0.));
#15086=DIRECTION('',(0.,1.,0.));
#15087=DIRECTION('center_axis',(0.,-1.,0.));
#15088=DIRECTION('ref_axis',(1.,0.,0.));
#15089=DIRECTION('center_axis',(0.,1.,0.));
#15090=DIRECTION('ref_axis',(1.,0.,0.));
#15091=DIRECTION('center_axis',(0.,1.,0.));
#15092=DIRECTION('ref_axis',(1.,0.,0.));
#15093=DIRECTION('',(0.,1.,0.));
#15094=DIRECTION('center_axis',(0.,-1.,0.));
#15095=DIRECTION('ref_axis',(1.,0.,0.));
#15096=DIRECTION('center_axis',(0.,1.,0.));
#15097=DIRECTION('ref_axis',(1.,0.,0.));
#15098=DIRECTION('center_axis',(0.,1.,0.));
#15099=DIRECTION('ref_axis',(1.,0.,0.));
#15100=DIRECTION('',(0.,1.,0.));
#15101=DIRECTION('center_axis',(0.,-1.,0.));
#15102=DIRECTION('ref_axis',(1.,0.,0.));
#15103=DIRECTION('center_axis',(0.,1.,0.));
#15104=DIRECTION('ref_axis',(1.,0.,0.));
#15105=DIRECTION('center_axis',(0.,1.,0.));
#15106=DIRECTION('ref_axis',(1.,0.,0.));
#15107=DIRECTION('',(0.,1.,0.));
#15108=DIRECTION('center_axis',(0.,-1.,0.));
#15109=DIRECTION('ref_axis',(1.,0.,0.));
#15110=DIRECTION('center_axis',(0.,0.,1.));
#15111=DIRECTION('ref_axis',(1.,0.,0.));
#15112=DIRECTION('center_axis',(0.,0.,1.));
#15113=DIRECTION('ref_axis',(1.,0.,0.));
#15114=DIRECTION('',(0.,0.,1.));
#15115=DIRECTION('center_axis',(0.,0.,-1.));
#15116=DIRECTION('ref_axis',(1.,0.,0.));
#15117=DIRECTION('center_axis',(0.,0.,1.));
#15118=DIRECTION('ref_axis',(1.,0.,0.));
#15119=DIRECTION('center_axis',(0.,0.,1.));
#15120=DIRECTION('ref_axis',(1.,0.,0.));
#15121=DIRECTION('',(0.,0.,1.));
#15122=DIRECTION('center_axis',(0.,0.,-1.));
#15123=DIRECTION('ref_axis',(1.,0.,0.));
#15124=DIRECTION('center_axis',(0.,1.,0.));
#15125=DIRECTION('ref_axis',(1.,0.,0.));
#15126=DIRECTION('center_axis',(0.,1.,0.));
#15127=DIRECTION('ref_axis',(1.,0.,0.));
#15128=DIRECTION('',(0.,1.,0.));
#15129=DIRECTION('center_axis',(0.,-1.,0.));
#15130=DIRECTION('ref_axis',(1.,0.,0.));
#15131=DIRECTION('center_axis',(0.,0.,1.));
#15132=DIRECTION('ref_axis',(1.,0.,0.));
#15133=DIRECTION('',(0.,1.,0.));
#15134=DIRECTION('',(-1.,0.,0.));
#15135=DIRECTION('',(0.,1.,0.));
#15136=DIRECTION('',(1.,0.,0.));
#15137=DIRECTION('center_axis',(0.,0.,1.));
#15138=DIRECTION('ref_axis',(1.,0.,0.));
#15139=DIRECTION('',(0.,-1.,0.));
#15140=DIRECTION('',(1.,0.,0.));
#15141=DIRECTION('',(0.,1.,0.));
#15142=DIRECTION('',(-1.,0.,0.));
#15143=DIRECTION('center_axis',(-1.,0.,0.));
#15144=DIRECTION('ref_axis',(0.,0.,1.));
#15145=DIRECTION('',(0.,0.,-1.));
#15146=DIRECTION('',(0.,0.,1.));
#15147=DIRECTION('',(0.,1.,0.));
#15148=DIRECTION('center_axis',(1.,0.,0.));
#15149=DIRECTION('ref_axis',(0.,0.,-1.));
#15150=DIRECTION('',(0.,0.,1.));
#15151=DIRECTION('',(0.,1.,0.));
#15152=DIRECTION('',(0.,0.,-1.));
#15153=DIRECTION('center_axis',(0.,-1.,0.));
#15154=DIRECTION('ref_axis',(1.,0.,0.));
#15155=DIRECTION('',(0.,0.,1.));
#15156=DIRECTION('',(1.,0.,0.));
#15157=DIRECTION('',(0.,0.,1.));
#15158=DIRECTION('',(1.,0.,0.));
#15159=DIRECTION('center_axis',(1.,0.,0.));
#15160=DIRECTION('ref_axis',(0.,1.,0.));
#15161=DIRECTION('',(0.,0.,1.));
#15162=DIRECTION('',(0.,1.,0.));
#15163=DIRECTION('center_axis',(0.,1.,0.));
#15164=DIRECTION('ref_axis',(-1.,0.,0.));
#15165=DIRECTION('',(0.,0.,1.));
#15166=DIRECTION('',(-1.,0.,0.));
#15167=DIRECTION('',(-1.,0.,0.));
#15168=DIRECTION('center_axis',(-1.,0.,0.));
#15169=DIRECTION('ref_axis',(0.,-1.,0.));
#15170=DIRECTION('',(0.,-1.,0.));
#15171=DIRECTION('center_axis',(0.,0.,1.));
#15172=DIRECTION('ref_axis',(1.,0.,0.));
#15173=DIRECTION('center_axis',(0.,0.,1.));
#15174=DIRECTION('ref_axis',(1.,0.,0.));
#15175=DIRECTION('axis',(0.,0.,1.));
#15176=DIRECTION('refdir',(1.,0.,0.));
#15177=DIRECTION('center_axis',(0.,1.,0.));
#15178=DIRECTION('ref_axis',(1.,0.,0.));
#15179=DIRECTION('center_axis',(0.,1.,0.));
#15180=DIRECTION('ref_axis',(1.,0.,0.));
#15181=DIRECTION('',(0.,1.,0.));
#15182=DIRECTION('center_axis',(0.,-1.,0.));
#15183=DIRECTION('ref_axis',(1.,0.,0.));
#15184=DIRECTION('center_axis',(0.,1.,0.));
#15185=DIRECTION('ref_axis',(1.,0.,0.));
#15186=DIRECTION('center_axis',(0.,1.,0.));
#15187=DIRECTION('ref_axis',(1.,0.,0.));
#15188=DIRECTION('',(0.,1.,0.));
#15189=DIRECTION('center_axis',(0.,-1.,0.));
#15190=DIRECTION('ref_axis',(1.,0.,0.));
#15191=DIRECTION('center_axis',(0.,1.,0.));
#15192=DIRECTION('ref_axis',(1.,0.,0.));
#15193=DIRECTION('center_axis',(0.,1.,0.));
#15194=DIRECTION('ref_axis',(1.,0.,0.));
#15195=DIRECTION('',(0.,1.,0.));
#15196=DIRECTION('center_axis',(0.,-1.,0.));
#15197=DIRECTION('ref_axis',(1.,0.,0.));
#15198=DIRECTION('center_axis',(0.,1.,0.));
#15199=DIRECTION('ref_axis',(1.,0.,0.));
#15200=DIRECTION('center_axis',(0.,1.,0.));
#15201=DIRECTION('ref_axis',(1.,0.,0.));
#15202=DIRECTION('',(0.,1.,0.));
#15203=DIRECTION('center_axis',(0.,-1.,0.));
#15204=DIRECTION('ref_axis',(1.,0.,0.));
#15205=DIRECTION('center_axis',(0.,1.,0.));
#15206=DIRECTION('ref_axis',(1.,0.,0.));
#15207=DIRECTION('center_axis',(0.,1.,0.));
#15208=DIRECTION('ref_axis',(1.,0.,0.));
#15209=DIRECTION('',(0.,-1.,0.));
#15210=DIRECTION('center_axis',(0.,-1.,0.));
#15211=DIRECTION('ref_axis',(1.,0.,0.));
#15212=DIRECTION('center_axis',(0.,1.,0.));
#15213=DIRECTION('ref_axis',(1.,0.,0.));
#15214=DIRECTION('center_axis',(0.,-1.,0.));
#15215=DIRECTION('ref_axis',(1.,0.,0.));
#15216=DIRECTION('center_axis',(0.,1.,0.));
#15217=DIRECTION('ref_axis',(1.,0.,0.));
#15218=DIRECTION('',(0.,-1.,0.));
#15219=DIRECTION('center_axis',(0.,-1.,0.));
#15220=DIRECTION('ref_axis',(1.,0.,0.));
#15221=DIRECTION('center_axis',(0.,1.,0.));
#15222=DIRECTION('ref_axis',(1.,0.,0.));
#15223=DIRECTION('center_axis',(0.,1.,0.));
#15224=DIRECTION('ref_axis',(1.,0.,0.));
#15225=DIRECTION('',(0.,-1.,0.));
#15226=DIRECTION('center_axis',(0.,1.,0.));
#15227=DIRECTION('ref_axis',(1.,0.,0.));
#15228=DIRECTION('center_axis',(0.,1.,0.));
#15229=DIRECTION('ref_axis',(1.,0.,0.));
#15230=DIRECTION('center_axis',(0.,1.,0.));
#15231=DIRECTION('ref_axis',(1.,0.,0.));
#15232=DIRECTION('axis',(0.,0.,1.));
#15233=DIRECTION('refdir',(1.,0.,0.));
#15234=DIRECTION('center_axis',(0.,1.,0.));
#15235=DIRECTION('ref_axis',(1.,0.,0.));
#15236=DIRECTION('center_axis',(0.,1.,0.));
#15237=DIRECTION('ref_axis',(1.,0.,0.));
#15238=DIRECTION('',(0.,1.,0.));
#15239=DIRECTION('center_axis',(0.,-1.,0.));
#15240=DIRECTION('ref_axis',(1.,0.,0.));
#15241=DIRECTION('center_axis',(0.,1.,0.));
#15242=DIRECTION('ref_axis',(1.,0.,0.));
#15243=DIRECTION('center_axis',(0.,1.,0.));
#15244=DIRECTION('ref_axis',(1.,0.,0.));
#15245=DIRECTION('',(0.,1.,0.));
#15246=DIRECTION('center_axis',(0.,-1.,0.));
#15247=DIRECTION('ref_axis',(1.,0.,0.));
#15248=DIRECTION('center_axis',(0.,1.,0.));
#15249=DIRECTION('ref_axis',(1.,0.,0.));
#15250=DIRECTION('center_axis',(0.,1.,0.));
#15251=DIRECTION('ref_axis',(1.,0.,0.));
#15252=DIRECTION('',(0.,1.,0.));
#15253=DIRECTION('center_axis',(0.,-1.,0.));
#15254=DIRECTION('ref_axis',(1.,0.,0.));
#15255=DIRECTION('center_axis',(0.,1.,0.));
#15256=DIRECTION('ref_axis',(1.,0.,0.));
#15257=DIRECTION('center_axis',(0.,1.,0.));
#15258=DIRECTION('ref_axis',(1.,0.,0.));
#15259=DIRECTION('',(0.,1.,0.));
#15260=DIRECTION('center_axis',(0.,-1.,0.));
#15261=DIRECTION('ref_axis',(1.,0.,0.));
#15262=DIRECTION('center_axis',(0.,1.,0.));
#15263=DIRECTION('ref_axis',(1.,0.,0.));
#15264=DIRECTION('center_axis',(0.,1.,0.));
#15265=DIRECTION('ref_axis',(1.,0.,0.));
#15266=DIRECTION('',(0.,-1.,0.));
#15267=DIRECTION('center_axis',(0.,1.,0.));
#15268=DIRECTION('ref_axis',(1.,0.,0.));
#15269=DIRECTION('center_axis',(0.,1.,0.));
#15270=DIRECTION('ref_axis',(1.,0.,0.));
#15271=DIRECTION('center_axis',(0.,-1.,0.));
#15272=DIRECTION('ref_axis',(1.,0.,0.));
#15273=DIRECTION('center_axis',(0.,1.,0.));
#15274=DIRECTION('ref_axis',(1.,0.,0.));
#15275=DIRECTION('center_axis',(0.,-1.,0.));
#15276=DIRECTION('ref_axis',(1.,0.,0.));
#15277=DIRECTION('',(0.,-1.,0.));
#15278=DIRECTION('center_axis',(0.,1.,0.));
#15279=DIRECTION('ref_axis',(1.,0.,0.));
#15280=DIRECTION('center_axis',(0.,1.,0.));
#15281=DIRECTION('ref_axis',(1.,0.,0.));
#15282=DIRECTION('',(0.,-1.,0.));
#15283=DIRECTION('center_axis',(0.,1.,0.));
#15284=DIRECTION('ref_axis',(1.,0.,0.));
#15285=DIRECTION('center_axis',(0.,1.,0.));
#15286=DIRECTION('ref_axis',(1.,0.,0.));
#15287=DIRECTION('center_axis',(0.,1.,0.));
#15288=DIRECTION('ref_axis',(1.,0.,0.));
#15289=DIRECTION('axis',(0.,0.,1.));
#15290=DIRECTION('refdir',(1.,0.,0.));
#15291=DIRECTION('center_axis',(0.,1.,0.));
#15292=DIRECTION('ref_axis',(1.,0.,0.));
#15293=DIRECTION('center_axis',(0.,1.,0.));
#15294=DIRECTION('ref_axis',(1.,0.,0.));
#15295=DIRECTION('',(0.,1.,0.));
#15296=DIRECTION('center_axis',(0.,-1.,0.));
#15297=DIRECTION('ref_axis',(1.,0.,0.));
#15298=DIRECTION('center_axis',(0.,1.,0.));
#15299=DIRECTION('ref_axis',(1.,0.,0.));
#15300=DIRECTION('center_axis',(0.,1.,0.));
#15301=DIRECTION('ref_axis',(1.,0.,0.));
#15302=DIRECTION('',(0.,1.,0.));
#15303=DIRECTION('center_axis',(0.,-1.,0.));
#15304=DIRECTION('ref_axis',(1.,0.,0.));
#15305=DIRECTION('center_axis',(0.,1.,0.));
#15306=DIRECTION('ref_axis',(1.,0.,0.));
#15307=DIRECTION('center_axis',(0.,1.,0.));
#15308=DIRECTION('ref_axis',(1.,0.,0.));
#15309=DIRECTION('',(0.,1.,0.));
#15310=DIRECTION('center_axis',(0.,-1.,0.));
#15311=DIRECTION('ref_axis',(1.,0.,0.));
#15312=DIRECTION('center_axis',(0.,1.,0.));
#15313=DIRECTION('ref_axis',(1.,0.,0.));
#15314=DIRECTION('center_axis',(0.,1.,0.));
#15315=DIRECTION('ref_axis',(1.,0.,0.));
#15316=DIRECTION('',(0.,1.,0.));
#15317=DIRECTION('center_axis',(0.,-1.,0.));
#15318=DIRECTION('ref_axis',(1.,0.,0.));
#15319=DIRECTION('center_axis',(0.,0.,1.));
#15320=DIRECTION('ref_axis',(1.,0.,0.));
#15321=DIRECTION('center_axis',(0.,0.,1.));
#15322=DIRECTION('ref_axis',(1.,0.,0.));
#15323=DIRECTION('',(0.,0.,1.));
#15324=DIRECTION('center_axis',(0.,0.,-1.));
#15325=DIRECTION('ref_axis',(1.,0.,0.));
#15326=DIRECTION('center_axis',(0.,0.,1.));
#15327=DIRECTION('ref_axis',(1.,0.,0.));
#15328=DIRECTION('center_axis',(0.,0.,1.));
#15329=DIRECTION('ref_axis',(1.,0.,0.));
#15330=DIRECTION('',(0.,0.,1.));
#15331=DIRECTION('center_axis',(0.,0.,-1.));
#15332=DIRECTION('ref_axis',(1.,0.,0.));
#15333=DIRECTION('center_axis',(0.,1.,0.));
#15334=DIRECTION('ref_axis',(1.,0.,0.));
#15335=DIRECTION('center_axis',(0.,1.,0.));
#15336=DIRECTION('ref_axis',(1.,0.,0.));
#15337=DIRECTION('',(0.,1.,0.));
#15338=DIRECTION('center_axis',(0.,-1.,0.));
#15339=DIRECTION('ref_axis',(1.,0.,0.));
#15340=DIRECTION('center_axis',(0.,0.,1.));
#15341=DIRECTION('ref_axis',(1.,0.,0.));
#15342=DIRECTION('',(0.,1.,0.));
#15343=DIRECTION('',(-1.,0.,0.));
#15344=DIRECTION('',(0.,1.,0.));
#15345=DIRECTION('',(1.,0.,0.));
#15346=DIRECTION('center_axis',(0.,0.,1.));
#15347=DIRECTION('ref_axis',(1.,0.,0.));
#15348=DIRECTION('',(0.,-1.,0.));
#15349=DIRECTION('',(1.,0.,0.));
#15350=DIRECTION('',(0.,1.,0.));
#15351=DIRECTION('',(-1.,0.,0.));
#15352=DIRECTION('center_axis',(-1.,0.,0.));
#15353=DIRECTION('ref_axis',(0.,0.,1.));
#15354=DIRECTION('',(0.,0.,-1.));
#15355=DIRECTION('',(0.,0.,1.));
#15356=DIRECTION('',(0.,1.,0.));
#15357=DIRECTION('center_axis',(1.,0.,0.));
#15358=DIRECTION('ref_axis',(0.,0.,-1.));
#15359=DIRECTION('',(0.,0.,1.));
#15360=DIRECTION('',(0.,1.,0.));
#15361=DIRECTION('',(0.,0.,-1.));
#15362=DIRECTION('center_axis',(0.,-1.,0.));
#15363=DIRECTION('ref_axis',(1.,0.,0.));
#15364=DIRECTION('',(0.,0.,1.));
#15365=DIRECTION('',(1.,0.,0.));
#15366=DIRECTION('',(0.,0.,1.));
#15367=DIRECTION('',(1.,0.,0.));
#15368=DIRECTION('center_axis',(1.,0.,0.));
#15369=DIRECTION('ref_axis',(0.,1.,0.));
#15370=DIRECTION('',(0.,0.,1.));
#15371=DIRECTION('',(0.,1.,0.));
#15372=DIRECTION('center_axis',(0.,1.,0.));
#15373=DIRECTION('ref_axis',(-1.,0.,0.));
#15374=DIRECTION('',(0.,0.,1.));
#15375=DIRECTION('',(-1.,0.,0.));
#15376=DIRECTION('',(-1.,0.,0.));
#15377=DIRECTION('center_axis',(-1.,0.,0.));
#15378=DIRECTION('ref_axis',(0.,-1.,0.));
#15379=DIRECTION('',(0.,-1.,0.));
#15380=DIRECTION('center_axis',(0.,0.,1.));
#15381=DIRECTION('ref_axis',(1.,0.,0.));
#15382=DIRECTION('center_axis',(0.,0.,1.));
#15383=DIRECTION('ref_axis',(1.,0.,0.));
#15384=DIRECTION('axis',(0.,0.,1.));
#15385=DIRECTION('refdir',(1.,0.,0.));
#15386=DIRECTION('center_axis',(0.,1.,0.));
#15387=DIRECTION('ref_axis',(1.,0.,0.));
#15388=DIRECTION('center_axis',(0.,1.,0.));
#15389=DIRECTION('ref_axis',(1.,0.,0.));
#15390=DIRECTION('',(0.,1.,0.));
#15391=DIRECTION('center_axis',(0.,-1.,0.));
#15392=DIRECTION('ref_axis',(1.,0.,0.));
#15393=DIRECTION('center_axis',(0.,1.,0.));
#15394=DIRECTION('ref_axis',(1.,0.,0.));
#15395=DIRECTION('center_axis',(0.,1.,0.));
#15396=DIRECTION('ref_axis',(1.,0.,0.));
#15397=DIRECTION('',(0.,1.,0.));
#15398=DIRECTION('center_axis',(0.,-1.,0.));
#15399=DIRECTION('ref_axis',(1.,0.,0.));
#15400=DIRECTION('center_axis',(0.,1.,0.));
#15401=DIRECTION('ref_axis',(1.,0.,0.));
#15402=DIRECTION('center_axis',(0.,1.,0.));
#15403=DIRECTION('ref_axis',(1.,0.,0.));
#15404=DIRECTION('',(0.,1.,0.));
#15405=DIRECTION('center_axis',(0.,-1.,0.));
#15406=DIRECTION('ref_axis',(1.,0.,0.));
#15407=DIRECTION('center_axis',(0.,1.,0.));
#15408=DIRECTION('ref_axis',(1.,0.,0.));
#15409=DIRECTION('center_axis',(0.,1.,0.));
#15410=DIRECTION('ref_axis',(1.,0.,0.));
#15411=DIRECTION('',(0.,1.,0.));
#15412=DIRECTION('center_axis',(0.,-1.,0.));
#15413=DIRECTION('ref_axis',(1.,0.,0.));
#15414=DIRECTION('center_axis',(0.,1.,0.));
#15415=DIRECTION('ref_axis',(1.,0.,0.));
#15416=DIRECTION('center_axis',(0.,1.,0.));
#15417=DIRECTION('ref_axis',(1.,0.,0.));
#15418=DIRECTION('',(0.,-1.,0.));
#15419=DIRECTION('center_axis',(0.,-1.,0.));
#15420=DIRECTION('ref_axis',(1.,0.,0.));
#15421=DIRECTION('center_axis',(0.,1.,0.));
#15422=DIRECTION('ref_axis',(1.,0.,0.));
#15423=DIRECTION('center_axis',(0.,-1.,0.));
#15424=DIRECTION('ref_axis',(1.,0.,0.));
#15425=DIRECTION('center_axis',(0.,1.,0.));
#15426=DIRECTION('ref_axis',(1.,0.,0.));
#15427=DIRECTION('',(0.,-1.,0.));
#15428=DIRECTION('center_axis',(0.,-1.,0.));
#15429=DIRECTION('ref_axis',(1.,0.,0.));
#15430=DIRECTION('center_axis',(0.,1.,0.));
#15431=DIRECTION('ref_axis',(1.,0.,0.));
#15432=DIRECTION('center_axis',(0.,1.,0.));
#15433=DIRECTION('ref_axis',(1.,0.,0.));
#15434=DIRECTION('',(0.,-1.,0.));
#15435=DIRECTION('center_axis',(0.,1.,0.));
#15436=DIRECTION('ref_axis',(1.,0.,0.));
#15437=DIRECTION('center_axis',(0.,1.,0.));
#15438=DIRECTION('ref_axis',(1.,0.,0.));
#15439=DIRECTION('center_axis',(0.,1.,0.));
#15440=DIRECTION('ref_axis',(1.,0.,0.));
#15441=DIRECTION('axis',(0.,0.,1.));
#15442=DIRECTION('refdir',(1.,0.,0.));
#15443=DIRECTION('center_axis',(0.,1.,0.));
#15444=DIRECTION('ref_axis',(1.,0.,0.));
#15445=DIRECTION('center_axis',(0.,1.,0.));
#15446=DIRECTION('ref_axis',(1.,0.,0.));
#15447=DIRECTION('',(0.,1.,0.));
#15448=DIRECTION('center_axis',(0.,-1.,0.));
#15449=DIRECTION('ref_axis',(1.,0.,0.));
#15450=DIRECTION('center_axis',(0.,1.,0.));
#15451=DIRECTION('ref_axis',(1.,0.,0.));
#15452=DIRECTION('center_axis',(0.,1.,0.));
#15453=DIRECTION('ref_axis',(1.,0.,0.));
#15454=DIRECTION('',(0.,1.,0.));
#15455=DIRECTION('center_axis',(0.,-1.,0.));
#15456=DIRECTION('ref_axis',(1.,0.,0.));
#15457=DIRECTION('center_axis',(0.,1.,0.));
#15458=DIRECTION('ref_axis',(1.,0.,0.));
#15459=DIRECTION('center_axis',(0.,1.,0.));
#15460=DIRECTION('ref_axis',(1.,0.,0.));
#15461=DIRECTION('',(0.,1.,0.));
#15462=DIRECTION('center_axis',(0.,-1.,0.));
#15463=DIRECTION('ref_axis',(1.,0.,0.));
#15464=DIRECTION('center_axis',(0.,1.,0.));
#15465=DIRECTION('ref_axis',(1.,0.,0.));
#15466=DIRECTION('center_axis',(0.,1.,0.));
#15467=DIRECTION('ref_axis',(1.,0.,0.));
#15468=DIRECTION('',(0.,1.,0.));
#15469=DIRECTION('center_axis',(0.,-1.,0.));
#15470=DIRECTION('ref_axis',(1.,0.,0.));
#15471=DIRECTION('center_axis',(0.,1.,0.));
#15472=DIRECTION('ref_axis',(1.,0.,0.));
#15473=DIRECTION('center_axis',(0.,1.,0.));
#15474=DIRECTION('ref_axis',(1.,0.,0.));
#15475=DIRECTION('',(0.,-1.,0.));
#15476=DIRECTION('center_axis',(0.,1.,0.));
#15477=DIRECTION('ref_axis',(1.,0.,0.));
#15478=DIRECTION('center_axis',(0.,1.,0.));
#15479=DIRECTION('ref_axis',(1.,0.,0.));
#15480=DIRECTION('center_axis',(0.,-1.,0.));
#15481=DIRECTION('ref_axis',(1.,0.,0.));
#15482=DIRECTION('center_axis',(0.,1.,0.));
#15483=DIRECTION('ref_axis',(1.,0.,0.));
#15484=DIRECTION('center_axis',(0.,-1.,0.));
#15485=DIRECTION('ref_axis',(1.,0.,0.));
#15486=DIRECTION('',(0.,-1.,0.));
#15487=DIRECTION('center_axis',(0.,1.,0.));
#15488=DIRECTION('ref_axis',(1.,0.,0.));
#15489=DIRECTION('center_axis',(0.,1.,0.));
#15490=DIRECTION('ref_axis',(1.,0.,0.));
#15491=DIRECTION('',(0.,-1.,0.));
#15492=DIRECTION('center_axis',(0.,1.,0.));
#15493=DIRECTION('ref_axis',(1.,0.,0.));
#15494=DIRECTION('center_axis',(0.,1.,0.));
#15495=DIRECTION('ref_axis',(1.,0.,0.));
#15496=DIRECTION('center_axis',(0.,1.,0.));
#15497=DIRECTION('ref_axis',(1.,0.,0.));
#15498=DIRECTION('axis',(0.,0.,1.));
#15499=DIRECTION('refdir',(1.,0.,0.));
#15500=DIRECTION('center_axis',(1.,0.,0.));
#15501=DIRECTION('ref_axis',(0.,0.,-1.));
#15502=DIRECTION('center_axis',(-1.,0.,0.));
#15503=DIRECTION('ref_axis',(0.,0.,-1.));
#15504=DIRECTION('center_axis',(1.,0.,0.));
#15505=DIRECTION('ref_axis',(0.,0.,-1.));
#15506=DIRECTION('center_axis',(-1.,0.,0.));
#15507=DIRECTION('ref_axis',(0.,0.,-1.));
#15508=DIRECTION('',(-0.707106781186548,8.65956056235493E-17,-0.707106781186547));
#15509=DIRECTION('center_axis',(1.,0.,0.));
#15510=DIRECTION('ref_axis',(0.,0.,-1.));
#15511=DIRECTION('center_axis',(1.,0.,0.));
#15512=DIRECTION('ref_axis',(0.,0.,-1.));
#15513=DIRECTION('',(-1.,0.,0.));
#15514=DIRECTION('center_axis',(1.,0.,0.));
#15515=DIRECTION('ref_axis',(0.,0.,-1.));
#15516=DIRECTION('axis',(0.,0.,1.));
#15517=DIRECTION('refdir',(1.,0.,0.));
#15518=DIRECTION('axis',(0.,0.,1.));
#15519=DIRECTION('refdir',(1.,0.,0.));
#15520=DIRECTION('center_axis',(0.,-1.,0.));
#15521=DIRECTION('ref_axis',(0.,0.,-1.));
#15522=DIRECTION('center_axis',(0.,-1.,0.));
#15523=DIRECTION('ref_axis',(1.,0.,0.));
#15524=DIRECTION('center_axis',(0.,-1.,0.));
#15525=DIRECTION('ref_axis',(1.,0.,0.));
#15526=DIRECTION('center_axis',(1.,0.,1.22464679914735E-16));
#15527=DIRECTION('ref_axis',(-1.22464679914735E-16,0.,1.));
#15528=DIRECTION('center_axis',(0.,1.,0.));
#15529=DIRECTION('ref_axis',(1.,0.,0.));
#15530=DIRECTION('center_axis',(0.,1.,0.));
#15531=DIRECTION('ref_axis',(1.,0.,0.));
#15532=DIRECTION('center_axis',(0.,-1.,0.));
#15533=DIRECTION('ref_axis',(1.,0.,0.));
#15534=DIRECTION('',(0.,1.,0.));
#15535=DIRECTION('center_axis',(0.,-1.,0.));
#15536=DIRECTION('ref_axis',(1.,0.,0.));
#15537=DIRECTION('center_axis',(0.,-1.,0.));
#15538=DIRECTION('ref_axis',(1.,0.,0.));
#15539=DIRECTION('center_axis',(0.,-1.,0.));
#15540=DIRECTION('ref_axis',(1.,0.,0.));
#15541=DIRECTION('',(0.,1.,0.));
#15542=DIRECTION('center_axis',(0.,-1.,0.));
#15543=DIRECTION('ref_axis',(1.,0.,0.));
#15544=DIRECTION('center_axis',(0.,1.,0.));
#15545=DIRECTION('ref_axis',(1.,0.,0.));
#15546=DIRECTION('',(-0.707106781186548,0.707106781186547,-8.65956056235493E-17));
#15547=DIRECTION('center_axis',(0.,-1.,0.));
#15548=DIRECTION('ref_axis',(1.,0.,0.));
#15549=DIRECTION('center_axis',(0.,1.,0.));
#15550=DIRECTION('ref_axis',(0.,0.,1.));
#15551=DIRECTION('center_axis',(0.,-1.,0.));
#15552=DIRECTION('ref_axis',(1.,0.,0.));
#15553=DIRECTION('center_axis',(0.,-1.,0.));
#15554=DIRECTION('ref_axis',(1.,0.,0.));
#15555=DIRECTION('',(0.,1.,0.));
#15556=DIRECTION('center_axis',(0.,-1.,0.));
#15557=DIRECTION('ref_axis',(0.,0.,-1.));
#15558=DIRECTION('center_axis',(0.,-1.,0.));
#15559=DIRECTION('ref_axis',(1.,0.,0.));
#15560=DIRECTION('center_axis',(0.,-1.,0.));
#15561=DIRECTION('ref_axis',(1.,0.,0.));
#15562=DIRECTION('',(0.707106781186548,0.707106781186547,8.65956056235493E-17));
#15563=DIRECTION('axis',(0.,0.,1.));
#15564=DIRECTION('refdir',(1.,0.,0.));
#15565=DIRECTION('center_axis',(0.,-1.,0.));
#15566=DIRECTION('ref_axis',(0.,0.,-1.));
#15567=DIRECTION('center_axis',(0.,-1.,0.));
#15568=DIRECTION('ref_axis',(1.,0.,0.));
#15569=DIRECTION('center_axis',(0.,-1.,0.));
#15570=DIRECTION('ref_axis',(1.,0.,0.));
#15571=DIRECTION('center_axis',(1.,0.,1.22464679914735E-16));
#15572=DIRECTION('ref_axis',(-1.22464679914735E-16,0.,1.));
#15573=DIRECTION('center_axis',(0.,1.,0.));
#15574=DIRECTION('ref_axis',(1.,0.,0.));
#15575=DIRECTION('center_axis',(0.,1.,0.));
#15576=DIRECTION('ref_axis',(1.,0.,0.));
#15577=DIRECTION('center_axis',(0.,-1.,0.));
#15578=DIRECTION('ref_axis',(1.,0.,0.));
#15579=DIRECTION('center_axis',(0.,-1.,0.));
#15580=DIRECTION('ref_axis',(1.,0.,0.));
#15581=DIRECTION('',(0.,1.,0.));
#15582=DIRECTION('center_axis',(0.,1.,0.));
#15583=DIRECTION('ref_axis',(0.,0.,1.));
#15584=DIRECTION('center_axis',(0.,-1.,0.));
#15585=DIRECTION('ref_axis',(1.,0.,0.));
#15586=DIRECTION('center_axis',(0.,-1.,0.));
#15587=DIRECTION('ref_axis',(1.,0.,0.));
#15588=DIRECTION('center_axis',(0.,-1.,0.));
#15589=DIRECTION('ref_axis',(1.,0.,0.));
#15590=DIRECTION('center_axis',(0.,-1.,0.));
#15591=DIRECTION('ref_axis',(1.,0.,0.));
#15592=DIRECTION('',(0.707106781186548,0.707106781186547,8.65956056235494E-17));
#15593=DIRECTION('center_axis',(0.,-1.,0.));
#15594=DIRECTION('ref_axis',(1.,0.,0.));
#15595=DIRECTION('center_axis',(0.,-1.,0.));
#15596=DIRECTION('ref_axis',(1.,0.,0.));
#15597=DIRECTION('',(0.,1.,0.));
#15598=DIRECTION('center_axis',(0.,1.,0.));
#15599=DIRECTION('ref_axis',(1.,0.,0.));
#15600=DIRECTION('center_axis',(0.,-1.,0.));
#15601=DIRECTION('ref_axis',(1.,0.,0.));
#15602=DIRECTION('',(-0.707106781186548,0.707106781186547,-8.65956056235494E-17));
#15603=DIRECTION('center_axis',(0.,-1.,0.));
#15604=DIRECTION('ref_axis',(0.,0.,-1.));
#15605=DIRECTION('center_axis',(0.,-1.,0.));
#15606=DIRECTION('ref_axis',(1.,0.,0.));
#15607=DIRECTION('',(0.,1.,0.));
#15608=DIRECTION('axis',(0.,0.,1.));
#15609=DIRECTION('refdir',(1.,0.,0.));
#15610=DIRECTION('center_axis',(0.,0.,1.));
#15611=DIRECTION('ref_axis',(1.,0.,0.));
#15612=DIRECTION('center_axis',(1.22464679914735E-16,-1.,0.));
#15613=DIRECTION('ref_axis',(-1.,-1.22464679914735E-16,0.));
#15614=DIRECTION('center_axis',(0.78183148246803,0.,0.623489801858733));
#15615=DIRECTION('ref_axis',(0.623489801858734,0.,-0.78183148246803));
#15616=DIRECTION('center_axis',(7.63554790147315E-17,-1.,-9.57467422477103E-17));
#15617=DIRECTION('ref_axis',(-0.623489801858734,-1.22464679914735E-16,0.78183148246803));
#15618=DIRECTION('center_axis',(0.974927912181824,0.,-0.222520933956314));
#15619=DIRECTION('ref_axis',(-0.222520933956314,0.,-0.974927912181824));
#15620=DIRECTION('center_axis',(-2.7250954951288E-17,-1.,-1.19394234705288E-16));
#15621=DIRECTION('ref_axis',(0.222520933956314,-1.22464679914735E-16,0.974927912181824));
#15622=DIRECTION('center_axis',(0.433883739117558,0.,-0.900968867902419));
#15623=DIRECTION('ref_axis',(-0.900968867902419,0.,-0.433883739117558));
#15624=DIRECTION('center_axis',(-1.10336864020811E-16,-1.,-5.31354332312403E-17));
#15625=DIRECTION('ref_axis',(0.900968867902419,-1.22464679914735E-16,0.433883739117558));
#15626=DIRECTION('center_axis',(-0.433883739117558,0.,-0.900968867902419));
#15627=DIRECTION('ref_axis',(-0.900968867902419,0.,0.433883739117558));
#15628=DIRECTION('center_axis',(-1.10336864020811E-16,-1.,5.31354332312403E-17));
#15629=DIRECTION('ref_axis',(0.900968867902419,-1.22464679914735E-16,-0.433883739117558));
#15630=DIRECTION('center_axis',(-0.974927912181824,0.,-0.222520933956314));
#15631=DIRECTION('ref_axis',(-0.222520933956315,0.,0.974927912181824));
#15632=DIRECTION('center_axis',(-2.7250954951288E-17,-1.,1.19394234705288E-16));
#15633=DIRECTION('ref_axis',(0.222520933956315,-1.22464679914735E-16,-0.974927912181824));
#15634=DIRECTION('center_axis',(-0.78183148246803,0.,0.623489801858734));
#15635=DIRECTION('ref_axis',(0.623489801858733,0.,0.78183148246803));
#15636=DIRECTION('center_axis',(7.63554790147315E-17,-1.,9.57467422477103E-17));
#15637=DIRECTION('ref_axis',(-0.623489801858733,-1.22464679914735E-16,-0.78183148246803));
#15638=DIRECTION('axis',(0.,0.,1.));
#15639=DIRECTION('refdir',(1.,0.,0.));
#15640=DIRECTION('center_axis',(0.,0.,1.));
#15641=DIRECTION('ref_axis',(1.,0.,0.));
#15642=DIRECTION('center_axis',(0.,-1.,0.));
#15643=DIRECTION('ref_axis',(0.,0.,-1.));
#15644=DIRECTION('center_axis',(0.,-1.,0.));
#15645=DIRECTION('ref_axis',(0.,0.,-1.));
#15646=DIRECTION('center_axis',(0.,1.,0.));
#15647=DIRECTION('ref_axis',(1.,0.,0.));
#15648=DIRECTION('center_axis',(0.,1.,0.));
#15649=DIRECTION('ref_axis',(1.,0.,0.));
#15650=DIRECTION('center_axis',(0.,1.,0.));
#15651=DIRECTION('ref_axis',(1.,0.,0.));
#15652=DIRECTION('center_axis',(0.,1.,0.));
#15653=DIRECTION('ref_axis',(1.,0.,0.));
#15654=DIRECTION('',(0.,-1.,0.));
#15655=DIRECTION('center_axis',(0.,-1.,0.));
#15656=DIRECTION('ref_axis',(1.,0.,0.));
#15657=DIRECTION('center_axis',(0.,1.,0.));
#15658=DIRECTION('ref_axis',(1.,0.,0.));
#15659=DIRECTION('center_axis',(0.,1.,0.));
#15660=DIRECTION('ref_axis',(1.,0.,0.));
#15661=DIRECTION('center_axis',(0.,1.,0.));
#15662=DIRECTION('ref_axis',(1.,0.,0.));
#15663=DIRECTION('center_axis',(0.,1.,0.));
#15664=DIRECTION('ref_axis',(1.,0.,0.));
#15665=DIRECTION('center_axis',(0.,1.,0.));
#15666=DIRECTION('ref_axis',(1.,0.,0.));
#15667=DIRECTION('center_axis',(0.,1.,0.));
#15668=DIRECTION('ref_axis',(1.,0.,0.));
#15669=DIRECTION('center_axis',(0.,-1.,0.));
#15670=DIRECTION('ref_axis',(1.,0.,0.));
#15671=DIRECTION('center_axis',(0.,-1.,0.));
#15672=DIRECTION('ref_axis',(0.,0.,-1.));
#15673=DIRECTION('center_axis',(8.96625347776458E-17,0.,1.));
#15674=DIRECTION('ref_axis',(1.,0.,0.));
#15675=DIRECTION('center_axis',(0.,-1.,0.));
#15676=DIRECTION('ref_axis',(0.,0.,-1.));
#15677=DIRECTION('center_axis',(0.,1.,0.));
#15678=DIRECTION('ref_axis',(1.,0.,0.));
#15679=DIRECTION('center_axis',(0.,-1.,0.));
#15680=DIRECTION('ref_axis',(1.,0.,0.));
#15681=DIRECTION('center_axis',(0.,-1.,0.));
#15682=DIRECTION('ref_axis',(0.,0.,-1.));
#15683=DIRECTION('center_axis',(0.,0.,1.));
#15684=DIRECTION('ref_axis',(1.,0.,0.));
#15685=DIRECTION('center_axis',(0.,-1.,0.));
#15686=DIRECTION('ref_axis',(0.,0.,-1.));
#15687=DIRECTION('center_axis',(0.,1.,0.));
#15688=DIRECTION('ref_axis',(1.,0.,0.));
#15689=DIRECTION('center_axis',(0.,-1.,0.));
#15690=DIRECTION('ref_axis',(1.,0.,0.));
#15691=DIRECTION('center_axis',(0.,-1.,0.));
#15692=DIRECTION('ref_axis',(1.,0.,0.));
#15693=DIRECTION('center_axis',(0.,-1.,0.));
#15694=DIRECTION('ref_axis',(0.,0.,-1.));
#15695=DIRECTION('center_axis',(0.,0.,1.));
#15696=DIRECTION('ref_axis',(1.,0.,0.));
#15697=DIRECTION('center_axis',(0.,-1.,0.));
#15698=DIRECTION('ref_axis',(0.,0.,-1.));
#15699=DIRECTION('center_axis',(0.,1.,0.));
#15700=DIRECTION('ref_axis',(1.,0.,0.));
#15701=DIRECTION('center_axis',(0.,-1.,0.));
#15702=DIRECTION('ref_axis',(1.,0.,0.));
#15703=DIRECTION('center_axis',(0.,-1.,0.));
#15704=DIRECTION('ref_axis',(0.,0.,-1.));
#15705=DIRECTION('center_axis',(8.96625347776458E-17,0.,1.));
#15706=DIRECTION('ref_axis',(1.,0.,0.));
#15707=DIRECTION('center_axis',(0.,-1.,0.));
#15708=DIRECTION('ref_axis',(0.,0.,-1.));
#15709=DIRECTION('center_axis',(0.,1.,0.));
#15710=DIRECTION('ref_axis',(1.,0.,0.));
#15711=DIRECTION('center_axis',(0.,-1.,0.));
#15712=DIRECTION('ref_axis',(1.,0.,0.));
#15713=DIRECTION('center_axis',(0.,-1.,0.));
#15714=DIRECTION('ref_axis',(0.,0.,-1.));
#15715=DIRECTION('center_axis',(0.,0.,1.));
#15716=DIRECTION('ref_axis',(1.,0.,0.));
#15717=DIRECTION('center_axis',(0.,-1.,0.));
#15718=DIRECTION('ref_axis',(0.,0.,-1.));
#15719=DIRECTION('center_axis',(0.,1.,0.));
#15720=DIRECTION('ref_axis',(1.,0.,0.));
#15721=DIRECTION('center_axis',(0.,1.,0.));
#15722=DIRECTION('ref_axis',(1.,0.,0.));
#15723=DIRECTION('',(0.,1.,0.));
#15724=DIRECTION('center_axis',(0.,-1.,0.));
#15725=DIRECTION('ref_axis',(1.,0.,0.));
#15726=DIRECTION('center_axis',(0.,-1.,0.));
#15727=DIRECTION('ref_axis',(1.,0.,0.));
#15728=DIRECTION('center_axis',(0.,1.,0.));
#15729=DIRECTION('ref_axis',(1.,0.,0.));
#15730=DIRECTION('center_axis',(0.,-1.,0.));
#15731=DIRECTION('ref_axis',(0.,0.,-1.));
#15732=DIRECTION('center_axis',(0.,0.,1.));
#15733=DIRECTION('ref_axis',(1.,0.,0.));
#15734=DIRECTION('center_axis',(0.,-1.,0.));
#15735=DIRECTION('ref_axis',(0.,0.,-1.));
#15736=DIRECTION('center_axis',(0.,-1.,0.));
#15737=DIRECTION('ref_axis',(-1.,0.,0.));
#15738=DIRECTION('center_axis',(0.,1.,0.));
#15739=DIRECTION('ref_axis',(1.,0.,0.));
#15740=DIRECTION('axis',(0.,0.,1.));
#15741=DIRECTION('refdir',(1.,0.,0.));
#15742=DIRECTION('center_axis',(0.,1.,0.));
#15743=DIRECTION('ref_axis',(0.,0.,1.));
#15744=DIRECTION('center_axis',(0.,-1.,0.));
#15745=DIRECTION('ref_axis',(1.,0.,0.));
#15746=DIRECTION('center_axis',(0.,-1.,0.));
#15747=DIRECTION('ref_axis',(1.,0.,0.));
#15748=DIRECTION('center_axis',(0.,-1.,0.));
#15749=DIRECTION('ref_axis',(1.,0.,0.));
#15750=DIRECTION('center_axis',(0.,-1.,0.));
#15751=DIRECTION('ref_axis',(1.,0.,0.));
#15752=DIRECTION('',(0.,1.,0.));
#15753=DIRECTION('center_axis',(0.,-1.,0.));
#15754=DIRECTION('ref_axis',(0.,0.,-1.));
#15755=DIRECTION('center_axis',(0.,-1.,0.));
#15756=DIRECTION('ref_axis',(1.,0.,0.));
#15757=DIRECTION('center_axis',(0.,-1.,0.));
#15758=DIRECTION('ref_axis',(1.,0.,0.));
#15759=DIRECTION('',(0.,1.,0.));
#15760=DIRECTION('center_axis',(0.,1.,0.));
#15761=DIRECTION('ref_axis',(0.,0.,1.));
#15762=DIRECTION('center_axis',(0.,-1.,0.));
#15763=DIRECTION('ref_axis',(1.,0.,0.));
#15764=DIRECTION('center_axis',(0.,-1.,0.));
#15765=DIRECTION('ref_axis',(1.,0.,0.));
#15766=DIRECTION('center_axis',(0.,-1.,0.));
#15767=DIRECTION('ref_axis',(1.,0.,0.));
#15768=DIRECTION('center_axis',(0.,-1.,0.));
#15769=DIRECTION('ref_axis',(1.,0.,0.));
#15770=DIRECTION('',(0.,1.,0.));
#15771=DIRECTION('center_axis',(0.,-1.,0.));
#15772=DIRECTION('ref_axis',(0.,0.,-1.));
#15773=DIRECTION('center_axis',(0.,-1.,0.));
#15774=DIRECTION('ref_axis',(1.,0.,0.));
#15775=DIRECTION('center_axis',(0.,-1.,0.));
#15776=DIRECTION('ref_axis',(1.,0.,0.));
#15777=DIRECTION('',(0.,1.,0.));
#15778=DIRECTION('',(0.,0.,1.));
#15779=DIRECTION('',(1.,0.,0.));
#15780=DIRECTION('',(0.,0.,1.));
#15781=DIRECTION('',(1.,0.,0.));
#15782=DIRECTION('',(0.,0.,1.));
#15783=DIRECTION('',(1.,0.,0.));
#15784=DIRECTION('',(0.,0.,1.));
#15785=DIRECTION('',(1.,0.,0.));
#15786=DIRECTION('',(0.,0.,1.));
#15787=DIRECTION('',(1.,0.,0.));
#15788=DIRECTION('axis',(0.,0.,1.));
#15789=DIRECTION('refdir',(1.,0.,0.));
#15790=DIRECTION('center_axis',(0.866025403784439,0.,-0.5));
#15791=DIRECTION('ref_axis',(0.5,0.,0.866025403784439));
#15792=DIRECTION('',(-0.5,0.,-0.866025403784439));
#15793=DIRECTION('',(0.,-1.,0.));
#15794=DIRECTION('',(0.5,0.,0.866025403784439));
#15795=DIRECTION('',(0.,-1.,0.));
#15796=DIRECTION('center_axis',(1.60246890531964E-16,0.,-1.));
#15797=DIRECTION('ref_axis',(1.,0.,1.60246890531964E-16));
#15798=DIRECTION('',(-1.,0.,-1.60246890531964E-16));
#15799=DIRECTION('',(0.,-1.,0.));
#15800=DIRECTION('',(1.,0.,1.60246890531964E-16));
#15801=DIRECTION('center_axis',(-0.866025403784439,0.,-0.5));
#15802=DIRECTION('ref_axis',(0.5,0.,-0.866025403784439));
#15803=DIRECTION('',(-0.5,0.,0.866025403784439));
#15804=DIRECTION('',(0.,-1.,0.));
#15805=DIRECTION('',(0.5,0.,-0.866025403784439));
#15806=DIRECTION('center_axis',(-0.866025403784439,0.,0.5));
#15807=DIRECTION('ref_axis',(-0.5,0.,-0.866025403784439));
#15808=DIRECTION('',(0.5,0.,0.866025403784439));
#15809=DIRECTION('',(0.,-1.,0.));
#15810=DIRECTION('',(-0.5,0.,-0.866025403784439));
#15811=DIRECTION('center_axis',(-1.60246890531964E-16,0.,1.));
#15812=DIRECTION('ref_axis',(-1.,0.,-1.60246890531964E-16));
#15813=DIRECTION('',(1.,0.,1.60246890531964E-16));
#15814=DIRECTION('',(0.,-1.,0.));
#15815=DIRECTION('',(-1.,0.,-1.60246890531964E-16));
#15816=DIRECTION('center_axis',(0.866025403784439,0.,0.5));
#15817=DIRECTION('ref_axis',(-0.5,0.,0.866025403784439));
#15818=DIRECTION('',(0.5,0.,-0.866025403784439));
#15819=DIRECTION('',(-0.5,0.,0.866025403784439));
#15820=DIRECTION('center_axis',(0.,1.,0.));
#15821=DIRECTION('ref_axis',(1.,0.,0.));
#15822=DIRECTION('center_axis',(0.,-1.,0.));
#15823=DIRECTION('ref_axis',(0.,0.,-1.));
#15824=DIRECTION('center_axis',(0.,1.,0.));
#15825=DIRECTION('ref_axis',(1.,0.,0.));
#15826=DIRECTION('center_axis',(0.,1.,0.));
#15827=DIRECTION('ref_axis',(1.,0.,0.));
#15828=DIRECTION('center_axis',(0.,1.,0.));
#15829=DIRECTION('ref_axis',(0.,0.,1.));
#15830=DIRECTION('center_axis',(0.,-1.,0.));
#15831=DIRECTION('ref_axis',(1.,0.,0.));
#15832=DIRECTION('center_axis',(0.,-1.,0.));
#15833=DIRECTION('ref_axis',(1.,0.,0.));
#15834=DIRECTION('center_axis',(0.,-1.,0.));
#15835=DIRECTION('ref_axis',(1.,0.,0.));
#15836=DIRECTION('',(0.707106781186547,0.707106781186548,8.65956056235493E-17));
#15837=DIRECTION('center_axis',(0.,-1.,0.));
#15838=DIRECTION('ref_axis',(1.,0.,0.));
#15839=DIRECTION('center_axis',(0.,-1.,0.));
#15840=DIRECTION('ref_axis',(1.,0.,0.));
#15841=DIRECTION('',(0.,1.,0.));
#15842=DIRECTION('center_axis',(0.,1.,0.));
#15843=DIRECTION('ref_axis',(1.,0.,0.));
#15844=DIRECTION('center_axis',(0.,-1.,0.));
#15845=DIRECTION('ref_axis',(1.,0.,0.));
#15846=DIRECTION('',(-0.707106781186547,0.707106781186548,-8.65956056235493E-17));
#15847=DIRECTION('center_axis',(0.,-1.,0.));
#15848=DIRECTION('ref_axis',(0.,0.,-1.));
#15849=DIRECTION('center_axis',(0.,-1.,0.));
#15850=DIRECTION('ref_axis',(1.,0.,0.));
#15851=DIRECTION('center_axis',(0.,1.,0.));
#15852=DIRECTION('ref_axis',(1.,0.,0.));
#15853=DIRECTION('center_axis',(0.,1.,0.));
#15854=DIRECTION('ref_axis',(1.,0.,0.));
#15855=DIRECTION('',(-0.447213595499958,0.894427190999916,-5.47678698264203E-17));
#15856=DIRECTION('center_axis',(0.,-1.,0.));
#15857=DIRECTION('ref_axis',(1.,0.,0.));
#15858=DIRECTION('',(0.,1.,0.));
#15859=DIRECTION('axis',(0.,0.,1.));
#15860=DIRECTION('refdir',(1.,0.,0.));
#15861=DIRECTION('axis',(0.,0.,1.));
#15862=DIRECTION('refdir',(1.,0.,0.));
#15863=DIRECTION('center_axis',(0.,0.,1.));
#15864=DIRECTION('ref_axis',(1.,0.,0.));
#15865=DIRECTION('center_axis',(0.,0.,1.));
#15866=DIRECTION('ref_axis',(1.,0.,0.));
#15867=DIRECTION('',(0.,0.,1.));
#15868=DIRECTION('center_axis',(0.,0.,1.));
#15869=DIRECTION('ref_axis',(1.,0.,0.));
#15870=DIRECTION('center_axis',(0.,0.,1.));
#15871=DIRECTION('ref_axis',(1.,0.,0.));
#15872=DIRECTION('center_axis',(1.,0.,0.));
#15873=DIRECTION('ref_axis',(0.,0.,-1.));
#15874=DIRECTION('',(0.,0.,-1.));
#15875=DIRECTION('',(0.,1.,0.));
#15876=DIRECTION('',(0.,0.,1.));
#15877=DIRECTION('',(0.,1.,0.));
#15878=DIRECTION('center_axis',(1.,0.,0.));
#15879=DIRECTION('ref_axis',(0.,0.,-1.));
#15880=DIRECTION('',(0.,0.,1.));
#15881=DIRECTION('',(0.,1.,0.));
#15882=DIRECTION('',(0.,0.,-1.));
#15883=DIRECTION('',(0.,1.,0.));
#15884=DIRECTION('center_axis',(0.,0.,-1.));
#15885=DIRECTION('ref_axis',(-1.,0.,0.));
#15886=DIRECTION('center_axis',(0.,0.,-1.));
#15887=DIRECTION('ref_axis',(1.,0.,0.));
#15888=DIRECTION('',(1.,0.,0.));
#15889=DIRECTION('',(0.,1.,0.));
#15890=DIRECTION('',(-1.,0.,0.));
#15891=DIRECTION('center_axis',(0.,0.,-1.));
#15892=DIRECTION('ref_axis',(1.,0.,0.));
#15893=DIRECTION('center_axis',(0.,0.,1.));
#15894=DIRECTION('ref_axis',(1.,0.,0.));
#15895=DIRECTION('center_axis',(0.,0.,1.));
#15896=DIRECTION('ref_axis',(1.,0.,0.));
#15897=DIRECTION('',(1.,0.,0.));
#15898=DIRECTION('',(0.,1.,0.));
#15899=DIRECTION('',(-1.,0.,0.));
#15900=DIRECTION('center_axis',(0.,0.,1.));
#15901=DIRECTION('ref_axis',(1.,0.,0.));
#15902=DIRECTION('center_axis',(-1.,0.,0.));
#15903=DIRECTION('ref_axis',(0.,0.,1.));
#15904=DIRECTION('',(0.,0.,-1.));
#15905=DIRECTION('',(0.,0.,1.));
#15906=DIRECTION('',(0.,1.,0.));
#15907=DIRECTION('center_axis',(-0.342020143325675,0.,0.939692620785906));
#15908=DIRECTION('ref_axis',(0.939692620785906,0.,0.342020143325675));
#15909=DIRECTION('',(-0.939692620785906,0.,-0.342020143325675));
#15910=DIRECTION('',(0.939692620785906,0.,0.342020143325675));
#15911=DIRECTION('',(0.,1.,0.));
#15912=DIRECTION('center_axis',(-1.,0.,0.));
#15913=DIRECTION('ref_axis',(0.,0.,1.));
#15914=DIRECTION('',(0.,0.,-1.));
#15915=DIRECTION('',(0.,0.,1.));
#15916=DIRECTION('',(0.,1.,0.));
#15917=DIRECTION('center_axis',(-0.342020143325675,0.,-0.939692620785906));
#15918=DIRECTION('ref_axis',(-0.939692620785906,0.,0.342020143325675));
#15919=DIRECTION('',(0.939692620785906,0.,-0.342020143325675));
#15920=DIRECTION('',(-0.939692620785906,0.,0.342020143325675));
#15921=DIRECTION('',(0.,1.,0.));
#15922=DIRECTION('center_axis',(-1.,0.,0.));
#15923=DIRECTION('ref_axis',(0.,0.,1.));
#15924=DIRECTION('',(0.,0.,-1.));
#15925=DIRECTION('',(0.,0.,1.));
#15926=DIRECTION('',(0.,1.,0.));
#15927=DIRECTION('center_axis',(-0.342020143325675,0.,0.939692620785906));
#15928=DIRECTION('ref_axis',(0.939692620785906,0.,0.342020143325675));
#15929=DIRECTION('',(-0.939692620785906,0.,-0.342020143325675));
#15930=DIRECTION('',(0.939692620785906,0.,0.342020143325675));
#15931=DIRECTION('',(0.,1.,0.));
#15932=DIRECTION('center_axis',(-1.,0.,0.));
#15933=DIRECTION('ref_axis',(0.,0.,1.));
#15934=DIRECTION('',(0.,0.,-1.));
#15935=DIRECTION('',(0.,0.,1.));
#15936=DIRECTION('',(0.,1.,0.));
#15937=DIRECTION('center_axis',(-0.342020143325675,0.,-0.939692620785906));
#15938=DIRECTION('ref_axis',(-0.939692620785906,0.,0.342020143325675));
#15939=DIRECTION('',(0.939692620785906,0.,-0.342020143325675));
#15940=DIRECTION('',(-0.939692620785906,0.,0.342020143325675));
#15941=DIRECTION('',(0.,1.,0.));
#15942=DIRECTION('center_axis',(-1.,0.,0.));
#15943=DIRECTION('ref_axis',(0.,0.,1.));
#15944=DIRECTION('',(0.,0.,-1.));
#15945=DIRECTION('',(0.,0.,1.));
#15946=DIRECTION('',(0.,1.,0.));
#15947=DIRECTION('center_axis',(-0.342020143325675,0.,0.939692620785906));
#15948=DIRECTION('ref_axis',(0.939692620785906,0.,0.342020143325675));
#15949=DIRECTION('',(-0.939692620785906,0.,-0.342020143325675));
#15950=DIRECTION('',(0.939692620785906,0.,0.342020143325675));
#15951=DIRECTION('',(0.,1.,0.));
#15952=DIRECTION('center_axis',(-1.,0.,0.));
#15953=DIRECTION('ref_axis',(0.,0.,1.));
#15954=DIRECTION('',(0.,0.,-1.));
#15955=DIRECTION('',(0.,0.,1.));
#15956=DIRECTION('',(0.,1.,0.));
#15957=DIRECTION('center_axis',(-0.342020143325675,0.,-0.939692620785906));
#15958=DIRECTION('ref_axis',(-0.939692620785906,0.,0.342020143325675));
#15959=DIRECTION('',(0.939692620785906,0.,-0.342020143325675));
#15960=DIRECTION('',(-0.939692620785906,0.,0.342020143325675));
#15961=DIRECTION('',(0.,1.,0.));
#15962=DIRECTION('center_axis',(-1.,0.,0.));
#15963=DIRECTION('ref_axis',(0.,0.,1.));
#15964=DIRECTION('',(0.,0.,-1.));
#15965=DIRECTION('',(0.,0.,1.));
#15966=DIRECTION('',(0.,1.,0.));
#15967=DIRECTION('center_axis',(-0.342020143325675,0.,0.939692620785906));
#15968=DIRECTION('ref_axis',(0.939692620785906,0.,0.342020143325675));
#15969=DIRECTION('',(-0.939692620785906,0.,-0.342020143325675));
#15970=DIRECTION('',(0.939692620785906,0.,0.342020143325675));
#15971=DIRECTION('',(0.,1.,0.));
#15972=DIRECTION('center_axis',(-1.,0.,0.));
#15973=DIRECTION('ref_axis',(0.,0.,1.));
#15974=DIRECTION('',(0.,0.,-1.));
#15975=DIRECTION('',(0.,0.,1.));
#15976=DIRECTION('',(0.,1.,0.));
#15977=DIRECTION('center_axis',(-0.342020143325675,0.,-0.939692620785906));
#15978=DIRECTION('ref_axis',(-0.939692620785906,0.,0.342020143325675));
#15979=DIRECTION('',(0.939692620785906,0.,-0.342020143325675));
#15980=DIRECTION('',(-0.939692620785906,0.,0.342020143325675));
#15981=DIRECTION('',(0.,1.,0.));
#15982=DIRECTION('center_axis',(-1.,0.,0.));
#15983=DIRECTION('ref_axis',(0.,0.,1.));
#15984=DIRECTION('',(0.,0.,-1.));
#15985=DIRECTION('',(0.,0.,1.));
#15986=DIRECTION('',(0.,1.,0.));
#15987=DIRECTION('center_axis',(-0.342020143325662,0.,0.939692620785911));
#15988=DIRECTION('ref_axis',(0.939692620785911,0.,0.342020143325662));
#15989=DIRECTION('',(-0.939692620785911,0.,-0.342020143325662));
#15990=DIRECTION('',(0.939692620785911,0.,0.342020143325662));
#15991=DIRECTION('',(0.,1.,0.));
#15992=DIRECTION('center_axis',(-1.,0.,0.));
#15993=DIRECTION('ref_axis',(0.,0.,1.));
#15994=DIRECTION('',(0.,0.,-1.));
#15995=DIRECTION('',(0.,0.,1.));
#15996=DIRECTION('',(0.,1.,0.));
#15997=DIRECTION('center_axis',(-0.342020143325662,0.,-0.939692620785911));
#15998=DIRECTION('ref_axis',(-0.939692620785911,0.,0.342020143325662));
#15999=DIRECTION('',(0.939692620785911,0.,-0.342020143325662));
#16000=DIRECTION('',(-0.939692620785911,0.,0.342020143325662));
#16001=DIRECTION('',(0.,1.,0.));
#16002=DIRECTION('center_axis',(-1.,0.,0.));
#16003=DIRECTION('ref_axis',(0.,0.,1.));
#16004=DIRECTION('',(0.,0.,-1.));
#16005=DIRECTION('',(0.,0.,1.));
#16006=DIRECTION('',(0.,1.,0.));
#16007=DIRECTION('center_axis',(-0.342020143325662,0.,0.939692620785911));
#16008=DIRECTION('ref_axis',(0.939692620785911,0.,0.342020143325662));
#16009=DIRECTION('',(-0.939692620785911,0.,-0.342020143325662));
#16010=DIRECTION('',(0.939692620785911,0.,0.342020143325662));
#16011=DIRECTION('',(0.,1.,0.));
#16012=DIRECTION('center_axis',(-1.,0.,0.));
#16013=DIRECTION('ref_axis',(0.,0.,1.));
#16014=DIRECTION('',(0.,0.,-1.));
#16015=DIRECTION('',(0.,0.,1.));
#16016=DIRECTION('',(0.,1.,0.));
#16017=DIRECTION('center_axis',(-0.342020143325662,0.,-0.939692620785911));
#16018=DIRECTION('ref_axis',(-0.939692620785911,0.,0.342020143325662));
#16019=DIRECTION('',(0.939692620785911,0.,-0.342020143325662));
#16020=DIRECTION('',(-0.939692620785911,0.,0.342020143325662));
#16021=DIRECTION('',(0.,1.,0.));
#16022=DIRECTION('center_axis',(-1.,0.,0.));
#16023=DIRECTION('ref_axis',(0.,0.,1.));
#16024=DIRECTION('',(0.,0.,-1.));
#16025=DIRECTION('',(0.,0.,1.));
#16026=DIRECTION('',(0.,1.,0.));
#16027=DIRECTION('center_axis',(-0.342020143325662,0.,0.939692620785911));
#16028=DIRECTION('ref_axis',(0.939692620785911,0.,0.342020143325662));
#16029=DIRECTION('',(-0.939692620785911,0.,-0.342020143325662));
#16030=DIRECTION('',(0.939692620785911,0.,0.342020143325662));
#16031=DIRECTION('',(0.,1.,0.));
#16032=DIRECTION('center_axis',(-1.,0.,0.));
#16033=DIRECTION('ref_axis',(0.,0.,1.));
#16034=DIRECTION('',(0.,0.,-1.));
#16035=DIRECTION('',(0.,0.,1.));
#16036=DIRECTION('',(0.,1.,0.));
#16037=DIRECTION('center_axis',(-0.342020143325662,0.,-0.939692620785911));
#16038=DIRECTION('ref_axis',(-0.939692620785911,0.,0.342020143325662));
#16039=DIRECTION('',(0.939692620785911,0.,-0.342020143325662));
#16040=DIRECTION('',(-0.939692620785911,0.,0.342020143325662));
#16041=DIRECTION('',(0.,1.,0.));
#16042=DIRECTION('center_axis',(-1.,0.,0.));
#16043=DIRECTION('ref_axis',(0.,0.,1.));
#16044=DIRECTION('',(0.,0.,-1.));
#16045=DIRECTION('',(0.,0.,1.));
#16046=DIRECTION('',(0.,1.,0.));
#16047=DIRECTION('center_axis',(-0.342020143325668,0.,0.939692620785909));
#16048=DIRECTION('ref_axis',(0.939692620785909,0.,0.342020143325668));
#16049=DIRECTION('',(-0.939692620785909,0.,-0.342020143325668));
#16050=DIRECTION('',(0.939692620785909,0.,0.342020143325668));
#16051=DIRECTION('',(0.,1.,0.));
#16052=DIRECTION('center_axis',(-1.,0.,0.));
#16053=DIRECTION('ref_axis',(0.,0.,1.));
#16054=DIRECTION('',(0.,0.,-1.));
#16055=DIRECTION('',(0.,0.,1.));
#16056=DIRECTION('',(0.,1.,0.));
#16057=DIRECTION('center_axis',(-0.342020143325668,0.,-0.939692620785909));
#16058=DIRECTION('ref_axis',(-0.939692620785909,0.,0.342020143325668));
#16059=DIRECTION('',(0.939692620785909,0.,-0.342020143325668));
#16060=DIRECTION('',(-0.939692620785909,0.,0.342020143325668));
#16061=DIRECTION('',(0.,1.,0.));
#16062=DIRECTION('center_axis',(-1.,0.,0.));
#16063=DIRECTION('ref_axis',(0.,0.,1.));
#16064=DIRECTION('',(0.,0.,-1.));
#16065=DIRECTION('',(0.,0.,1.));
#16066=DIRECTION('',(0.,1.,0.));
#16067=DIRECTION('center_axis',(-0.342020143325668,0.,0.939692620785909));
#16068=DIRECTION('ref_axis',(0.939692620785909,0.,0.342020143325668));
#16069=DIRECTION('',(-0.939692620785909,0.,-0.342020143325668));
#16070=DIRECTION('',(0.939692620785909,0.,0.342020143325668));
#16071=DIRECTION('',(0.,1.,0.));
#16072=DIRECTION('center_axis',(-1.,0.,0.));
#16073=DIRECTION('ref_axis',(0.,0.,1.));
#16074=DIRECTION('',(0.,0.,-1.));
#16075=DIRECTION('',(0.,0.,1.));
#16076=DIRECTION('',(0.,1.,0.));
#16077=DIRECTION('center_axis',(-0.342020143325668,0.,-0.939692620785909));
#16078=DIRECTION('ref_axis',(-0.939692620785909,0.,0.342020143325668));
#16079=DIRECTION('',(0.939692620785909,0.,-0.342020143325668));
#16080=DIRECTION('',(-0.939692620785909,0.,0.342020143325668));
#16081=DIRECTION('',(0.,1.,0.));
#16082=DIRECTION('center_axis',(-1.,0.,0.));
#16083=DIRECTION('ref_axis',(0.,0.,1.));
#16084=DIRECTION('',(0.,0.,-1.));
#16085=DIRECTION('',(0.,0.,1.));
#16086=DIRECTION('',(0.,1.,0.));
#16087=DIRECTION('center_axis',(-0.342020143325668,0.,0.939692620785909));
#16088=DIRECTION('ref_axis',(0.939692620785909,0.,0.342020143325668));
#16089=DIRECTION('',(-0.939692620785909,0.,-0.342020143325668));
#16090=DIRECTION('',(0.939692620785909,0.,0.342020143325668));
#16091=DIRECTION('',(0.,1.,0.));
#16092=DIRECTION('center_axis',(-1.,0.,0.));
#16093=DIRECTION('ref_axis',(0.,0.,1.));
#16094=DIRECTION('',(0.,0.,-1.));
#16095=DIRECTION('',(0.,0.,1.));
#16096=DIRECTION('',(0.,1.,0.));
#16097=DIRECTION('center_axis',(-0.342020143325668,0.,-0.939692620785909));
#16098=DIRECTION('ref_axis',(-0.939692620785909,0.,0.342020143325668));
#16099=DIRECTION('',(0.939692620785909,0.,-0.342020143325668));
#16100=DIRECTION('',(-0.939692620785909,0.,0.342020143325668));
#16101=DIRECTION('',(0.,1.,0.));
#16102=DIRECTION('center_axis',(-1.,0.,0.));
#16103=DIRECTION('ref_axis',(0.,0.,1.));
#16104=DIRECTION('',(0.,0.,-1.));
#16105=DIRECTION('',(0.,0.,1.));
#16106=DIRECTION('',(0.,1.,0.));
#16107=DIRECTION('center_axis',(-0.342020143325668,0.,0.939692620785909));
#16108=DIRECTION('ref_axis',(0.939692620785909,0.,0.342020143325668));
#16109=DIRECTION('',(-0.939692620785909,0.,-0.342020143325668));
#16110=DIRECTION('',(0.939692620785909,0.,0.342020143325668));
#16111=DIRECTION('',(0.,1.,0.));
#16112=DIRECTION('center_axis',(-1.,0.,0.));
#16113=DIRECTION('ref_axis',(0.,0.,1.));
#16114=DIRECTION('',(0.,0.,-1.));
#16115=DIRECTION('',(0.,0.,1.));
#16116=DIRECTION('',(0.,1.,0.));
#16117=DIRECTION('center_axis',(-0.342020143325668,0.,-0.939692620785909));
#16118=DIRECTION('ref_axis',(-0.939692620785909,0.,0.342020143325668));
#16119=DIRECTION('',(0.939692620785909,0.,-0.342020143325668));
#16120=DIRECTION('',(-0.939692620785909,0.,0.342020143325668));
#16121=DIRECTION('',(0.,1.,0.));
#16122=DIRECTION('center_axis',(-1.,0.,0.));
#16123=DIRECTION('ref_axis',(0.,0.,1.));
#16124=DIRECTION('',(0.,0.,-1.));
#16125=DIRECTION('',(0.,0.,1.));
#16126=DIRECTION('',(0.,1.,0.));
#16127=DIRECTION('center_axis',(-0.342020143325668,0.,0.939692620785909));
#16128=DIRECTION('ref_axis',(0.939692620785909,0.,0.342020143325668));
#16129=DIRECTION('',(-0.939692620785909,0.,-0.342020143325668));
#16130=DIRECTION('',(0.939692620785909,0.,0.342020143325668));
#16131=DIRECTION('',(0.,1.,0.));
#16132=DIRECTION('center_axis',(-1.,0.,0.));
#16133=DIRECTION('ref_axis',(0.,0.,1.));
#16134=DIRECTION('',(0.,0.,-1.));
#16135=DIRECTION('',(0.,0.,1.));
#16136=DIRECTION('',(0.,1.,0.));
#16137=DIRECTION('center_axis',(-0.342020143325668,0.,-0.939692620785909));
#16138=DIRECTION('ref_axis',(-0.939692620785909,0.,0.342020143325668));
#16139=DIRECTION('',(0.939692620785909,0.,-0.342020143325668));
#16140=DIRECTION('',(-0.939692620785909,0.,0.342020143325668));
#16141=DIRECTION('',(0.,1.,0.));
#16142=DIRECTION('center_axis',(-1.,0.,0.));
#16143=DIRECTION('ref_axis',(0.,0.,1.));
#16144=DIRECTION('',(0.,0.,-1.));
#16145=DIRECTION('',(0.,0.,1.));
#16146=DIRECTION('',(0.,1.,0.));
#16147=DIRECTION('center_axis',(-0.342020143325668,0.,0.939692620785909));
#16148=DIRECTION('ref_axis',(0.939692620785909,0.,0.342020143325668));
#16149=DIRECTION('',(-0.939692620785909,0.,-0.342020143325668));
#16150=DIRECTION('',(0.939692620785909,0.,0.342020143325668));
#16151=DIRECTION('',(0.,1.,0.));
#16152=DIRECTION('center_axis',(-1.,0.,0.));
#16153=DIRECTION('ref_axis',(0.,0.,1.));
#16154=DIRECTION('',(0.,0.,-1.));
#16155=DIRECTION('',(0.,0.,1.));
#16156=DIRECTION('',(0.,1.,0.));
#16157=DIRECTION('center_axis',(-0.342020143325668,0.,-0.939692620785909));
#16158=DIRECTION('ref_axis',(-0.939692620785909,0.,0.342020143325668));
#16159=DIRECTION('',(0.939692620785909,0.,-0.342020143325668));
#16160=DIRECTION('',(-0.939692620785909,0.,0.342020143325668));
#16161=DIRECTION('',(0.,1.,0.));
#16162=DIRECTION('center_axis',(-1.,0.,0.));
#16163=DIRECTION('ref_axis',(0.,0.,1.));
#16164=DIRECTION('',(0.,0.,-1.));
#16165=DIRECTION('',(0.,0.,1.));
#16166=DIRECTION('',(0.,1.,0.));
#16167=DIRECTION('center_axis',(-0.342020143325668,0.,0.939692620785909));
#16168=DIRECTION('ref_axis',(0.939692620785909,0.,0.342020143325668));
#16169=DIRECTION('',(-0.939692620785909,0.,-0.342020143325668));
#16170=DIRECTION('',(0.939692620785909,0.,0.342020143325668));
#16171=DIRECTION('',(0.,1.,0.));
#16172=DIRECTION('center_axis',(-1.,0.,0.));
#16173=DIRECTION('ref_axis',(0.,0.,1.));
#16174=DIRECTION('',(0.,0.,-1.));
#16175=DIRECTION('',(0.,0.,1.));
#16176=DIRECTION('',(0.,1.,0.));
#16177=DIRECTION('center_axis',(-0.342020143325668,0.,-0.939692620785909));
#16178=DIRECTION('ref_axis',(-0.939692620785909,0.,0.342020143325668));
#16179=DIRECTION('',(0.939692620785909,0.,-0.342020143325668));
#16180=DIRECTION('',(-0.939692620785909,0.,0.342020143325668));
#16181=DIRECTION('',(0.,1.,0.));
#16182=DIRECTION('center_axis',(-1.,0.,0.));
#16183=DIRECTION('ref_axis',(0.,0.,1.));
#16184=DIRECTION('',(0.,0.,-1.));
#16185=DIRECTION('',(0.,0.,1.));
#16186=DIRECTION('',(0.,1.,0.));
#16187=DIRECTION('center_axis',(-0.342020143325662,0.,0.939692620785911));
#16188=DIRECTION('ref_axis',(0.939692620785911,0.,0.342020143325662));
#16189=DIRECTION('',(-0.939692620785911,0.,-0.342020143325662));
#16190=DIRECTION('',(0.939692620785911,0.,0.342020143325662));
#16191=DIRECTION('',(0.,1.,0.));
#16192=DIRECTION('center_axis',(-1.,0.,0.));
#16193=DIRECTION('ref_axis',(0.,0.,1.));
#16194=DIRECTION('',(0.,0.,-1.));
#16195=DIRECTION('',(0.,0.,1.));
#16196=DIRECTION('',(0.,1.,0.));
#16197=DIRECTION('center_axis',(-0.342020143325662,0.,-0.939692620785911));
#16198=DIRECTION('ref_axis',(-0.939692620785911,0.,0.342020143325662));
#16199=DIRECTION('',(0.939692620785911,0.,-0.342020143325662));
#16200=DIRECTION('',(-0.939692620785911,0.,0.342020143325662));
#16201=DIRECTION('',(0.,1.,0.));
#16202=DIRECTION('center_axis',(-1.,0.,0.));
#16203=DIRECTION('ref_axis',(0.,0.,1.));
#16204=DIRECTION('',(0.,0.,-1.));
#16205=DIRECTION('',(0.,0.,1.));
#16206=DIRECTION('',(0.,1.,0.));
#16207=DIRECTION('center_axis',(-0.342020143325668,0.,0.939692620785909));
#16208=DIRECTION('ref_axis',(0.939692620785909,0.,0.342020143325668));
#16209=DIRECTION('',(-0.939692620785909,0.,-0.342020143325668));
#16210=DIRECTION('',(0.939692620785909,0.,0.342020143325668));
#16211=DIRECTION('',(0.,1.,0.));
#16212=DIRECTION('center_axis',(-1.,0.,0.));
#16213=DIRECTION('ref_axis',(0.,0.,1.));
#16214=DIRECTION('',(0.,0.,-1.));
#16215=DIRECTION('',(0.,0.,1.));
#16216=DIRECTION('',(0.,1.,0.));
#16217=DIRECTION('center_axis',(-0.342020143325668,0.,-0.939692620785909));
#16218=DIRECTION('ref_axis',(-0.939692620785909,0.,0.342020143325668));
#16219=DIRECTION('',(0.939692620785909,0.,-0.342020143325668));
#16220=DIRECTION('',(-0.939692620785909,0.,0.342020143325668));
#16221=DIRECTION('',(0.,1.,0.));
#16222=DIRECTION('center_axis',(-1.,0.,0.));
#16223=DIRECTION('ref_axis',(0.,0.,1.));
#16224=DIRECTION('',(0.,0.,-1.));
#16225=DIRECTION('',(0.,0.,1.));
#16226=DIRECTION('',(0.,1.,0.));
#16227=DIRECTION('center_axis',(-0.342020143325668,0.,0.939692620785909));
#16228=DIRECTION('ref_axis',(0.939692620785909,0.,0.342020143325668));
#16229=DIRECTION('',(-0.939692620785909,0.,-0.342020143325668));
#16230=DIRECTION('',(0.939692620785909,0.,0.342020143325668));
#16231=DIRECTION('',(0.,1.,0.));
#16232=DIRECTION('center_axis',(-1.,0.,0.));
#16233=DIRECTION('ref_axis',(0.,0.,1.));
#16234=DIRECTION('',(0.,0.,-1.));
#16235=DIRECTION('',(0.,0.,1.));
#16236=DIRECTION('',(0.,1.,0.));
#16237=DIRECTION('center_axis',(-0.342020143325668,0.,-0.939692620785909));
#16238=DIRECTION('ref_axis',(-0.939692620785909,0.,0.342020143325668));
#16239=DIRECTION('',(0.939692620785909,0.,-0.342020143325668));
#16240=DIRECTION('',(-0.939692620785909,0.,0.342020143325668));
#16241=DIRECTION('',(0.,1.,0.));
#16242=DIRECTION('center_axis',(-1.,0.,0.));
#16243=DIRECTION('ref_axis',(0.,0.,1.));
#16244=DIRECTION('',(0.,0.,-1.));
#16245=DIRECTION('',(0.,0.,1.));
#16246=DIRECTION('',(0.,1.,0.));
#16247=DIRECTION('center_axis',(-0.342020143325668,0.,0.939692620785909));
#16248=DIRECTION('ref_axis',(0.939692620785909,0.,0.342020143325668));
#16249=DIRECTION('',(-0.939692620785909,0.,-0.342020143325668));
#16250=DIRECTION('',(0.939692620785909,0.,0.342020143325668));
#16251=DIRECTION('',(0.,1.,0.));
#16252=DIRECTION('center_axis',(-1.,0.,0.));
#16253=DIRECTION('ref_axis',(0.,0.,1.));
#16254=DIRECTION('',(0.,0.,-1.));
#16255=DIRECTION('',(0.,0.,1.));
#16256=DIRECTION('',(0.,1.,0.));
#16257=DIRECTION('center_axis',(-0.342020143325662,0.,-0.939692620785911));
#16258=DIRECTION('ref_axis',(-0.939692620785911,0.,0.342020143325662));
#16259=DIRECTION('',(0.939692620785911,0.,-0.342020143325662));
#16260=DIRECTION('',(-0.939692620785911,0.,0.342020143325662));
#16261=DIRECTION('',(0.,1.,0.));
#16262=DIRECTION('center_axis',(-1.,0.,0.));
#16263=DIRECTION('ref_axis',(0.,0.,1.));
#16264=DIRECTION('',(0.,0.,-1.));
#16265=DIRECTION('',(0.,0.,1.));
#16266=DIRECTION('',(0.,1.,0.));
#16267=DIRECTION('center_axis',(-0.342020143325668,0.,0.939692620785909));
#16268=DIRECTION('ref_axis',(0.939692620785909,0.,0.342020143325668));
#16269=DIRECTION('',(-0.939692620785909,0.,-0.342020143325668));
#16270=DIRECTION('',(0.939692620785909,0.,0.342020143325668));
#16271=DIRECTION('',(0.,1.,0.));
#16272=DIRECTION('center_axis',(-1.,0.,0.));
#16273=DIRECTION('ref_axis',(0.,0.,1.));
#16274=DIRECTION('',(0.,0.,-1.));
#16275=DIRECTION('',(0.,0.,1.));
#16276=DIRECTION('',(0.,1.,0.));
#16277=DIRECTION('center_axis',(-0.342020143325668,0.,-0.939692620785909));
#16278=DIRECTION('ref_axis',(-0.939692620785909,0.,0.342020143325668));
#16279=DIRECTION('',(0.939692620785909,0.,-0.342020143325668));
#16280=DIRECTION('',(-0.939692620785909,0.,0.342020143325668));
#16281=DIRECTION('',(0.,1.,0.));
#16282=DIRECTION('center_axis',(-1.,0.,0.));
#16283=DIRECTION('ref_axis',(0.,0.,1.));
#16284=DIRECTION('',(0.,0.,-1.));
#16285=DIRECTION('',(0.,0.,1.));
#16286=DIRECTION('',(0.,1.,0.));
#16287=DIRECTION('center_axis',(-0.342020143325662,0.,0.939692620785911));
#16288=DIRECTION('ref_axis',(0.939692620785911,0.,0.342020143325662));
#16289=DIRECTION('',(-0.939692620785911,0.,-0.342020143325662));
#16290=DIRECTION('',(0.939692620785911,0.,0.342020143325662));
#16291=DIRECTION('',(0.,1.,0.));
#16292=DIRECTION('center_axis',(-1.,0.,0.));
#16293=DIRECTION('ref_axis',(0.,0.,1.));
#16294=DIRECTION('',(0.,0.,-1.));
#16295=DIRECTION('',(0.,0.,1.));
#16296=DIRECTION('',(0.,1.,0.));
#16297=DIRECTION('center_axis',(-0.342020143325668,0.,-0.939692620785909));
#16298=DIRECTION('ref_axis',(-0.939692620785909,0.,0.342020143325668));
#16299=DIRECTION('',(0.939692620785909,0.,-0.342020143325668));
#16300=DIRECTION('',(-0.939692620785909,0.,0.342020143325668));
#16301=DIRECTION('',(0.,1.,0.));
#16302=DIRECTION('center_axis',(-1.,0.,0.));
#16303=DIRECTION('ref_axis',(0.,0.,1.));
#16304=DIRECTION('',(0.,0.,-1.));
#16305=DIRECTION('',(0.,0.,1.));
#16306=DIRECTION('',(0.,1.,0.));
#16307=DIRECTION('center_axis',(-0.342020143325668,0.,0.939692620785909));
#16308=DIRECTION('ref_axis',(0.939692620785909,0.,0.342020143325668));
#16309=DIRECTION('',(-0.939692620785909,0.,-0.342020143325668));
#16310=DIRECTION('',(0.939692620785909,0.,0.342020143325668));
#16311=DIRECTION('',(0.,1.,0.));
#16312=DIRECTION('center_axis',(-1.,0.,0.));
#16313=DIRECTION('ref_axis',(0.,0.,1.));
#16314=DIRECTION('',(0.,0.,-1.));
#16315=DIRECTION('',(0.,0.,1.));
#16316=DIRECTION('',(0.,1.,0.));
#16317=DIRECTION('center_axis',(-0.342020143325668,0.,-0.939692620785909));
#16318=DIRECTION('ref_axis',(-0.939692620785909,0.,0.342020143325668));
#16319=DIRECTION('',(0.939692620785909,0.,-0.342020143325668));
#16320=DIRECTION('',(-0.939692620785909,0.,0.342020143325668));
#16321=DIRECTION('',(0.,1.,0.));
#16322=DIRECTION('center_axis',(-1.,0.,0.));
#16323=DIRECTION('ref_axis',(0.,0.,1.));
#16324=DIRECTION('',(0.,0.,-1.));
#16325=DIRECTION('',(0.,0.,1.));
#16326=DIRECTION('',(0.,1.,0.));
#16327=DIRECTION('center_axis',(-0.342020143325668,0.,0.939692620785909));
#16328=DIRECTION('ref_axis',(0.939692620785909,0.,0.342020143325668));
#16329=DIRECTION('',(-0.939692620785909,0.,-0.342020143325668));
#16330=DIRECTION('',(0.939692620785909,0.,0.342020143325668));
#16331=DIRECTION('',(0.,1.,0.));
#16332=DIRECTION('center_axis',(-1.,0.,0.));
#16333=DIRECTION('ref_axis',(0.,0.,1.));
#16334=DIRECTION('',(0.,0.,-1.));
#16335=DIRECTION('',(0.,0.,1.));
#16336=DIRECTION('',(0.,1.,0.));
#16337=DIRECTION('center_axis',(-0.342020143325662,0.,-0.939692620785911));
#16338=DIRECTION('ref_axis',(-0.939692620785911,0.,0.342020143325662));
#16339=DIRECTION('',(0.939692620785911,0.,-0.342020143325662));
#16340=DIRECTION('',(-0.939692620785911,0.,0.342020143325662));
#16341=DIRECTION('',(0.,1.,0.));
#16342=DIRECTION('center_axis',(-1.,0.,0.));
#16343=DIRECTION('ref_axis',(0.,0.,1.));
#16344=DIRECTION('',(0.,0.,-1.));
#16345=DIRECTION('',(0.,0.,1.));
#16346=DIRECTION('',(0.,1.,0.));
#16347=DIRECTION('center_axis',(-0.342020143325668,0.,0.939692620785909));
#16348=DIRECTION('ref_axis',(0.939692620785909,0.,0.342020143325668));
#16349=DIRECTION('',(-0.939692620785909,0.,-0.342020143325668));
#16350=DIRECTION('',(0.939692620785909,0.,0.342020143325668));
#16351=DIRECTION('',(0.,1.,0.));
#16352=DIRECTION('center_axis',(-1.,0.,0.));
#16353=DIRECTION('ref_axis',(0.,0.,1.));
#16354=DIRECTION('',(0.,0.,-1.));
#16355=DIRECTION('',(0.,0.,1.));
#16356=DIRECTION('',(0.,1.,0.));
#16357=DIRECTION('center_axis',(-0.342020143325668,0.,-0.939692620785909));
#16358=DIRECTION('ref_axis',(-0.939692620785909,0.,0.342020143325668));
#16359=DIRECTION('',(0.939692620785909,0.,-0.342020143325668));
#16360=DIRECTION('',(-0.939692620785909,0.,0.342020143325668));
#16361=DIRECTION('',(0.,1.,0.));
#16362=DIRECTION('center_axis',(-1.,0.,0.));
#16363=DIRECTION('ref_axis',(0.,0.,1.));
#16364=DIRECTION('',(0.,0.,-1.));
#16365=DIRECTION('',(0.,0.,1.));
#16366=DIRECTION('',(0.,1.,0.));
#16367=DIRECTION('center_axis',(-0.342020143325668,0.,0.939692620785909));
#16368=DIRECTION('ref_axis',(0.939692620785909,0.,0.342020143325668));
#16369=DIRECTION('',(-0.939692620785909,0.,-0.342020143325668));
#16370=DIRECTION('',(0.939692620785909,0.,0.342020143325668));
#16371=DIRECTION('',(0.,1.,0.));
#16372=DIRECTION('center_axis',(-1.,0.,0.));
#16373=DIRECTION('ref_axis',(0.,0.,1.));
#16374=DIRECTION('',(0.,0.,-1.));
#16375=DIRECTION('',(0.,0.,1.));
#16376=DIRECTION('',(0.,1.,0.));
#16377=DIRECTION('center_axis',(-0.342020143325668,0.,-0.939692620785909));
#16378=DIRECTION('ref_axis',(-0.939692620785909,0.,0.342020143325668));
#16379=DIRECTION('',(0.939692620785909,0.,-0.342020143325668));
#16380=DIRECTION('',(-0.939692620785909,0.,0.342020143325668));
#16381=DIRECTION('',(0.,1.,0.));
#16382=DIRECTION('center_axis',(-1.,0.,0.));
#16383=DIRECTION('ref_axis',(0.,0.,1.));
#16384=DIRECTION('',(0.,0.,-1.));
#16385=DIRECTION('',(0.,0.,1.));
#16386=DIRECTION('',(0.,1.,0.));
#16387=DIRECTION('center_axis',(-0.342020143325668,0.,0.939692620785909));
#16388=DIRECTION('ref_axis',(0.939692620785909,0.,0.342020143325668));
#16389=DIRECTION('',(-0.939692620785909,0.,-0.342020143325668));
#16390=DIRECTION('',(0.939692620785909,0.,0.342020143325668));
#16391=DIRECTION('',(0.,1.,0.));
#16392=DIRECTION('center_axis',(-1.,0.,0.));
#16393=DIRECTION('ref_axis',(0.,0.,1.));
#16394=DIRECTION('',(0.,0.,-1.));
#16395=DIRECTION('',(0.,0.,1.));
#16396=DIRECTION('',(0.,1.,0.));
#16397=DIRECTION('center_axis',(-0.342020143325668,0.,-0.939692620785909));
#16398=DIRECTION('ref_axis',(-0.939692620785909,0.,0.342020143325668));
#16399=DIRECTION('',(0.939692620785909,0.,-0.342020143325668));
#16400=DIRECTION('',(-0.939692620785909,0.,0.342020143325668));
#16401=DIRECTION('',(0.,1.,0.));
#16402=DIRECTION('center_axis',(-1.,0.,0.));
#16403=DIRECTION('ref_axis',(0.,0.,1.));
#16404=DIRECTION('',(0.,0.,-1.));
#16405=DIRECTION('',(0.,0.,1.));
#16406=DIRECTION('',(0.,1.,0.));
#16407=DIRECTION('center_axis',(-0.342020143325668,0.,0.939692620785909));
#16408=DIRECTION('ref_axis',(0.939692620785909,0.,0.342020143325668));
#16409=DIRECTION('',(-0.939692620785909,0.,-0.342020143325668));
#16410=DIRECTION('',(0.939692620785909,0.,0.342020143325668));
#16411=DIRECTION('',(0.,1.,0.));
#16412=DIRECTION('center_axis',(-1.,0.,0.));
#16413=DIRECTION('ref_axis',(0.,0.,1.));
#16414=DIRECTION('',(0.,0.,-1.));
#16415=DIRECTION('',(0.,0.,1.));
#16416=DIRECTION('',(0.,1.,0.));
#16417=DIRECTION('center_axis',(-0.342020143325662,0.,-0.939692620785911));
#16418=DIRECTION('ref_axis',(-0.939692620785911,0.,0.342020143325662));
#16419=DIRECTION('',(0.939692620785911,0.,-0.342020143325662));
#16420=DIRECTION('',(-0.939692620785911,0.,0.342020143325662));
#16421=DIRECTION('',(0.,1.,0.));
#16422=DIRECTION('center_axis',(-1.,0.,0.));
#16423=DIRECTION('ref_axis',(0.,0.,1.));
#16424=DIRECTION('',(0.,0.,-1.));
#16425=DIRECTION('',(0.,0.,1.));
#16426=DIRECTION('',(0.,1.,0.));
#16427=DIRECTION('center_axis',(-0.342020143325668,0.,0.939692620785909));
#16428=DIRECTION('ref_axis',(0.939692620785909,0.,0.342020143325668));
#16429=DIRECTION('',(-0.939692620785909,0.,-0.342020143325668));
#16430=DIRECTION('',(0.939692620785909,0.,0.342020143325668));
#16431=DIRECTION('',(0.,1.,0.));
#16432=DIRECTION('center_axis',(-1.,0.,0.));
#16433=DIRECTION('ref_axis',(0.,0.,1.));
#16434=DIRECTION('',(0.,0.,-1.));
#16435=DIRECTION('',(0.,0.,1.));
#16436=DIRECTION('',(0.,1.,0.));
#16437=DIRECTION('center_axis',(-0.342020143325668,0.,-0.939692620785909));
#16438=DIRECTION('ref_axis',(-0.939692620785909,0.,0.342020143325668));
#16439=DIRECTION('',(0.939692620785909,0.,-0.342020143325668));
#16440=DIRECTION('',(-0.939692620785909,0.,0.342020143325668));
#16441=DIRECTION('',(0.,1.,0.));
#16442=DIRECTION('center_axis',(-1.,0.,0.));
#16443=DIRECTION('ref_axis',(0.,0.,1.));
#16444=DIRECTION('',(0.,0.,-1.));
#16445=DIRECTION('',(0.,0.,1.));
#16446=DIRECTION('',(0.,1.,0.));
#16447=DIRECTION('center_axis',(-0.342020143325662,0.,0.939692620785911));
#16448=DIRECTION('ref_axis',(0.939692620785911,0.,0.342020143325662));
#16449=DIRECTION('',(-0.939692620785911,0.,-0.342020143325662));
#16450=DIRECTION('',(0.939692620785911,0.,0.342020143325662));
#16451=DIRECTION('',(0.,1.,0.));
#16452=DIRECTION('center_axis',(-1.,0.,0.));
#16453=DIRECTION('ref_axis',(0.,0.,1.));
#16454=DIRECTION('',(0.,0.,-1.));
#16455=DIRECTION('',(0.,0.,1.));
#16456=DIRECTION('',(0.,1.,0.));
#16457=DIRECTION('center_axis',(-0.342020143325668,0.,-0.939692620785909));
#16458=DIRECTION('ref_axis',(-0.939692620785909,0.,0.342020143325668));
#16459=DIRECTION('',(0.939692620785909,0.,-0.342020143325668));
#16460=DIRECTION('',(-0.939692620785909,0.,0.342020143325668));
#16461=DIRECTION('',(0.,1.,0.));
#16462=DIRECTION('center_axis',(-1.,0.,0.));
#16463=DIRECTION('ref_axis',(0.,0.,1.));
#16464=DIRECTION('',(0.,0.,-1.));
#16465=DIRECTION('',(0.,0.,1.));
#16466=DIRECTION('',(0.,1.,0.));
#16467=DIRECTION('center_axis',(-0.342020143325668,0.,0.939692620785909));
#16468=DIRECTION('ref_axis',(0.939692620785909,0.,0.342020143325668));
#16469=DIRECTION('',(-0.939692620785909,0.,-0.342020143325668));
#16470=DIRECTION('',(0.939692620785909,0.,0.342020143325668));
#16471=DIRECTION('',(0.,1.,0.));
#16472=DIRECTION('center_axis',(-1.,0.,0.));
#16473=DIRECTION('ref_axis',(0.,0.,1.));
#16474=DIRECTION('',(0.,0.,-1.));
#16475=DIRECTION('',(0.,0.,1.));
#16476=DIRECTION('',(0.,1.,0.));
#16477=DIRECTION('center_axis',(-0.342020143325668,0.,-0.939692620785909));
#16478=DIRECTION('ref_axis',(-0.939692620785909,0.,0.342020143325668));
#16479=DIRECTION('',(0.939692620785909,0.,-0.342020143325668));
#16480=DIRECTION('',(-0.939692620785909,0.,0.342020143325668));
#16481=DIRECTION('',(0.,1.,0.));
#16482=DIRECTION('center_axis',(-1.,0.,0.));
#16483=DIRECTION('ref_axis',(0.,0.,1.));
#16484=DIRECTION('',(0.,0.,-1.));
#16485=DIRECTION('',(0.,0.,1.));
#16486=DIRECTION('',(0.,1.,0.));
#16487=DIRECTION('center_axis',(-0.342020143325668,0.,0.939692620785909));
#16488=DIRECTION('ref_axis',(0.939692620785909,0.,0.342020143325668));
#16489=DIRECTION('',(-0.939692620785909,0.,-0.342020143325668));
#16490=DIRECTION('',(0.939692620785909,0.,0.342020143325668));
#16491=DIRECTION('',(0.,1.,0.));
#16492=DIRECTION('center_axis',(-1.,0.,0.));
#16493=DIRECTION('ref_axis',(0.,0.,1.));
#16494=DIRECTION('',(0.,0.,-1.));
#16495=DIRECTION('',(0.,0.,1.));
#16496=DIRECTION('',(0.,1.,0.));
#16497=DIRECTION('center_axis',(-0.342020143325662,0.,-0.939692620785911));
#16498=DIRECTION('ref_axis',(-0.939692620785911,0.,0.342020143325662));
#16499=DIRECTION('',(0.939692620785911,0.,-0.342020143325662));
#16500=DIRECTION('',(-0.939692620785911,0.,0.342020143325662));
#16501=DIRECTION('',(0.,1.,0.));
#16502=DIRECTION('center_axis',(-1.,0.,0.));
#16503=DIRECTION('ref_axis',(0.,0.,1.));
#16504=DIRECTION('',(0.,0.,-1.));
#16505=DIRECTION('',(0.,0.,1.));
#16506=DIRECTION('',(0.,1.,0.));
#16507=DIRECTION('center_axis',(-0.342020143325668,0.,0.939692620785909));
#16508=DIRECTION('ref_axis',(0.939692620785909,0.,0.342020143325668));
#16509=DIRECTION('',(-0.939692620785909,0.,-0.342020143325668));
#16510=DIRECTION('',(0.939692620785909,0.,0.342020143325668));
#16511=DIRECTION('',(0.,1.,0.));
#16512=DIRECTION('center_axis',(-1.,0.,0.));
#16513=DIRECTION('ref_axis',(0.,0.,1.));
#16514=DIRECTION('',(0.,0.,-1.));
#16515=DIRECTION('',(0.,0.,1.));
#16516=DIRECTION('',(0.,1.,0.));
#16517=DIRECTION('center_axis',(-0.342020143325668,0.,-0.939692620785909));
#16518=DIRECTION('ref_axis',(-0.939692620785909,0.,0.342020143325668));
#16519=DIRECTION('',(0.939692620785909,0.,-0.342020143325668));
#16520=DIRECTION('',(-0.939692620785909,0.,0.342020143325668));
#16521=DIRECTION('',(0.,1.,0.));
#16522=DIRECTION('center_axis',(-1.,0.,0.));
#16523=DIRECTION('ref_axis',(0.,0.,1.));
#16524=DIRECTION('',(0.,0.,-1.));
#16525=DIRECTION('',(0.,0.,1.));
#16526=DIRECTION('',(0.,1.,0.));
#16527=DIRECTION('center_axis',(-0.342020143325668,0.,0.939692620785909));
#16528=DIRECTION('ref_axis',(0.939692620785909,0.,0.342020143325668));
#16529=DIRECTION('',(-0.939692620785909,0.,-0.342020143325668));
#16530=DIRECTION('',(0.939692620785909,0.,0.342020143325668));
#16531=DIRECTION('',(0.,1.,0.));
#16532=DIRECTION('center_axis',(-1.,0.,0.));
#16533=DIRECTION('ref_axis',(0.,0.,1.));
#16534=DIRECTION('',(0.,0.,-1.));
#16535=DIRECTION('',(0.,0.,1.));
#16536=DIRECTION('',(0.,1.,0.));
#16537=DIRECTION('center_axis',(-0.342020143325668,0.,-0.939692620785909));
#16538=DIRECTION('ref_axis',(-0.939692620785909,0.,0.342020143325668));
#16539=DIRECTION('',(0.939692620785909,0.,-0.342020143325668));
#16540=DIRECTION('',(-0.939692620785909,0.,0.342020143325668));
#16541=DIRECTION('',(0.,1.,0.));
#16542=DIRECTION('center_axis',(-1.,0.,0.));
#16543=DIRECTION('ref_axis',(0.,0.,1.));
#16544=DIRECTION('',(0.,0.,-1.));
#16545=DIRECTION('',(0.,0.,1.));
#16546=DIRECTION('',(0.,1.,0.));
#16547=DIRECTION('center_axis',(-0.342020143325668,0.,0.939692620785909));
#16548=DIRECTION('ref_axis',(0.939692620785909,0.,0.342020143325668));
#16549=DIRECTION('',(-0.939692620785909,0.,-0.342020143325668));
#16550=DIRECTION('',(0.939692620785909,0.,0.342020143325668));
#16551=DIRECTION('',(0.,1.,0.));
#16552=DIRECTION('center_axis',(-1.,0.,0.));
#16553=DIRECTION('ref_axis',(0.,0.,1.));
#16554=DIRECTION('',(0.,0.,-1.));
#16555=DIRECTION('',(0.,0.,1.));
#16556=DIRECTION('',(0.,1.,0.));
#16557=DIRECTION('center_axis',(-0.342020143325665,0.,-0.93969262078591));
#16558=DIRECTION('ref_axis',(-0.93969262078591,0.,0.342020143325665));
#16559=DIRECTION('',(0.93969262078591,0.,-0.342020143325665));
#16560=DIRECTION('',(-0.93969262078591,0.,0.342020143325665));
#16561=DIRECTION('',(0.,1.,0.));
#16562=DIRECTION('center_axis',(-1.,0.,0.));
#16563=DIRECTION('ref_axis',(0.,0.,1.));
#16564=DIRECTION('',(0.,0.,-1.));
#16565=DIRECTION('',(0.,0.,1.));
#16566=DIRECTION('',(0.,1.,0.));
#16567=DIRECTION('center_axis',(-0.342020143325668,0.,0.939692620785909));
#16568=DIRECTION('ref_axis',(0.939692620785909,0.,0.342020143325668));
#16569=DIRECTION('',(-0.939692620785909,0.,-0.342020143325668));
#16570=DIRECTION('',(0.939692620785909,0.,0.342020143325668));
#16571=DIRECTION('',(0.,1.,0.));
#16572=DIRECTION('center_axis',(-1.,0.,0.));
#16573=DIRECTION('ref_axis',(0.,0.,1.));
#16574=DIRECTION('',(0.,0.,-1.));
#16575=DIRECTION('',(0.,0.,1.));
#16576=DIRECTION('',(0.,1.,0.));
#16577=DIRECTION('center_axis',(-0.342020143325668,0.,-0.939692620785909));
#16578=DIRECTION('ref_axis',(-0.939692620785909,0.,0.342020143325668));
#16579=DIRECTION('',(0.939692620785909,0.,-0.342020143325668));
#16580=DIRECTION('',(-0.939692620785909,0.,0.342020143325668));
#16581=DIRECTION('',(0.,1.,0.));
#16582=DIRECTION('center_axis',(-1.,0.,0.));
#16583=DIRECTION('ref_axis',(0.,0.,1.));
#16584=DIRECTION('',(0.,0.,-1.));
#16585=DIRECTION('',(0.,0.,1.));
#16586=DIRECTION('',(0.,1.,0.));
#16587=DIRECTION('center_axis',(-0.342020143325665,0.,0.93969262078591));
#16588=DIRECTION('ref_axis',(0.93969262078591,0.,0.342020143325665));
#16589=DIRECTION('',(-0.93969262078591,0.,-0.342020143325665));
#16590=DIRECTION('',(0.93969262078591,0.,0.342020143325665));
#16591=DIRECTION('',(0.,1.,0.));
#16592=DIRECTION('center_axis',(-1.,0.,0.));
#16593=DIRECTION('ref_axis',(0.,0.,1.));
#16594=DIRECTION('',(0.,0.,-1.));
#16595=DIRECTION('',(0.,0.,1.));
#16596=DIRECTION('',(0.,1.,0.));
#16597=DIRECTION('center_axis',(-0.342020143325665,0.,-0.93969262078591));
#16598=DIRECTION('ref_axis',(-0.93969262078591,0.,0.342020143325665));
#16599=DIRECTION('',(0.93969262078591,0.,-0.342020143325665));
#16600=DIRECTION('',(-0.93969262078591,0.,0.342020143325665));
#16601=DIRECTION('',(0.,1.,0.));
#16602=DIRECTION('center_axis',(-1.,0.,0.));
#16603=DIRECTION('ref_axis',(0.,0.,1.));
#16604=DIRECTION('',(0.,0.,-1.));
#16605=DIRECTION('',(0.,0.,1.));
#16606=DIRECTION('',(0.,1.,0.));
#16607=DIRECTION('center_axis',(-0.342020143325668,0.,0.939692620785909));
#16608=DIRECTION('ref_axis',(0.939692620785909,0.,0.342020143325668));
#16609=DIRECTION('',(-0.939692620785909,0.,-0.342020143325668));
#16610=DIRECTION('',(0.939692620785909,0.,0.342020143325668));
#16611=DIRECTION('',(0.,1.,0.));
#16612=DIRECTION('center_axis',(-1.,0.,0.));
#16613=DIRECTION('ref_axis',(0.,0.,1.));
#16614=DIRECTION('',(0.,0.,-1.));
#16615=DIRECTION('',(0.,0.,1.));
#16616=DIRECTION('',(0.,1.,0.));
#16617=DIRECTION('center_axis',(-0.342020143325668,0.,-0.939692620785909));
#16618=DIRECTION('ref_axis',(-0.939692620785909,0.,0.342020143325668));
#16619=DIRECTION('',(0.939692620785909,0.,-0.342020143325668));
#16620=DIRECTION('',(-0.939692620785909,0.,0.342020143325668));
#16621=DIRECTION('',(0.,1.,0.));
#16622=DIRECTION('center_axis',(-1.,0.,0.));
#16623=DIRECTION('ref_axis',(0.,0.,1.));
#16624=DIRECTION('',(0.,0.,-1.));
#16625=DIRECTION('',(0.,0.,1.));
#16626=DIRECTION('',(0.,1.,0.));
#16627=DIRECTION('center_axis',(-0.342020143325668,0.,0.939692620785909));
#16628=DIRECTION('ref_axis',(0.939692620785909,0.,0.342020143325668));
#16629=DIRECTION('',(-0.939692620785909,0.,-0.342020143325668));
#16630=DIRECTION('',(0.939692620785909,0.,0.342020143325668));
#16631=DIRECTION('',(0.,1.,0.));
#16632=DIRECTION('center_axis',(-1.,0.,0.));
#16633=DIRECTION('ref_axis',(0.,0.,1.));
#16634=DIRECTION('',(0.,0.,-1.));
#16635=DIRECTION('',(0.,0.,1.));
#16636=DIRECTION('',(0.,1.,0.));
#16637=DIRECTION('center_axis',(-0.342020143325665,0.,-0.93969262078591));
#16638=DIRECTION('ref_axis',(-0.93969262078591,0.,0.342020143325665));
#16639=DIRECTION('',(0.93969262078591,0.,-0.342020143325665));
#16640=DIRECTION('',(-0.93969262078591,0.,0.342020143325665));
#16641=DIRECTION('',(0.,1.,0.));
#16642=DIRECTION('center_axis',(-1.,0.,0.));
#16643=DIRECTION('ref_axis',(0.,0.,1.));
#16644=DIRECTION('',(0.,0.,-1.));
#16645=DIRECTION('',(0.,0.,1.));
#16646=DIRECTION('',(0.,1.,0.));
#16647=DIRECTION('center_axis',(-0.342020143325668,0.,0.939692620785909));
#16648=DIRECTION('ref_axis',(0.939692620785909,0.,0.342020143325668));
#16649=DIRECTION('',(-0.939692620785909,0.,-0.342020143325668));
#16650=DIRECTION('',(0.939692620785909,0.,0.342020143325668));
#16651=DIRECTION('',(0.,1.,0.));
#16652=DIRECTION('center_axis',(-1.,0.,0.));
#16653=DIRECTION('ref_axis',(0.,0.,1.));
#16654=DIRECTION('',(0.,0.,-1.));
#16655=DIRECTION('',(0.,0.,1.));
#16656=DIRECTION('',(0.,1.,0.));
#16657=DIRECTION('center_axis',(-0.342020143325671,0.,-0.939692620785907));
#16658=DIRECTION('ref_axis',(-0.939692620785907,0.,0.342020143325671));
#16659=DIRECTION('',(0.939692620785907,0.,-0.342020143325671));
#16660=DIRECTION('',(-0.939692620785907,0.,0.342020143325671));
#16661=DIRECTION('',(0.,1.,0.));
#16662=DIRECTION('center_axis',(-1.,0.,0.));
#16663=DIRECTION('ref_axis',(0.,0.,1.));
#16664=DIRECTION('',(0.,0.,-1.));
#16665=DIRECTION('',(0.,0.,1.));
#16666=DIRECTION('',(0.,1.,0.));
#16667=DIRECTION('center_axis',(-0.342020143325668,0.,0.939692620785909));
#16668=DIRECTION('ref_axis',(0.939692620785909,0.,0.342020143325668));
#16669=DIRECTION('',(-0.939692620785909,0.,-0.342020143325668));
#16670=DIRECTION('',(0.939692620785909,0.,0.342020143325668));
#16671=DIRECTION('',(0.,1.,0.));
#16672=DIRECTION('center_axis',(-1.,0.,0.));
#16673=DIRECTION('ref_axis',(0.,0.,1.));
#16674=DIRECTION('',(0.,0.,-1.));
#16675=DIRECTION('',(0.,0.,1.));
#16676=DIRECTION('',(0.,1.,0.));
#16677=DIRECTION('center_axis',(-0.342020143325668,0.,-0.939692620785909));
#16678=DIRECTION('ref_axis',(-0.939692620785909,0.,0.342020143325668));
#16679=DIRECTION('',(0.939692620785909,0.,-0.342020143325668));
#16680=DIRECTION('',(-0.939692620785909,0.,0.342020143325668));
#16681=DIRECTION('',(0.,1.,0.));
#16682=DIRECTION('center_axis',(-1.,0.,0.));
#16683=DIRECTION('ref_axis',(0.,0.,1.));
#16684=DIRECTION('',(0.,0.,-1.));
#16685=DIRECTION('',(0.,0.,1.));
#16686=DIRECTION('',(0.,1.,0.));
#16687=DIRECTION('center_axis',(-0.342020143325668,0.,0.939692620785909));
#16688=DIRECTION('ref_axis',(0.939692620785909,0.,0.342020143325668));
#16689=DIRECTION('',(-0.939692620785909,0.,-0.342020143325668));
#16690=DIRECTION('',(0.939692620785909,0.,0.342020143325668));
#16691=DIRECTION('',(0.,1.,0.));
#16692=DIRECTION('center_axis',(-1.,0.,0.));
#16693=DIRECTION('ref_axis',(0.,0.,1.));
#16694=DIRECTION('',(0.,0.,-1.));
#16695=DIRECTION('',(0.,0.,1.));
#16696=DIRECTION('',(0.,1.,0.));
#16697=DIRECTION('center_axis',(-0.342020143325671,0.,-0.939692620785907));
#16698=DIRECTION('ref_axis',(-0.939692620785907,0.,0.342020143325671));
#16699=DIRECTION('',(0.939692620785907,0.,-0.342020143325671));
#16700=DIRECTION('',(-0.939692620785907,0.,0.342020143325671));
#16701=DIRECTION('',(0.,1.,0.));
#16702=DIRECTION('center_axis',(-1.,0.,0.));
#16703=DIRECTION('ref_axis',(0.,0.,1.));
#16704=DIRECTION('',(0.,0.,-1.));
#16705=DIRECTION('',(0.,0.,1.));
#16706=DIRECTION('center_axis',(0.,1.,0.));
#16707=DIRECTION('ref_axis',(0.,0.,1.));
#16708=DIRECTION('center_axis',(0.,1.,0.));
#16709=DIRECTION('ref_axis',(1.,0.,0.));
#16710=DIRECTION('center_axis',(0.,0.,1.));
#16711=DIRECTION('ref_axis',(1.,0.,0.));
#16712=DIRECTION('center_axis',(0.,0.,1.));
#16713=DIRECTION('ref_axis',(1.,0.,0.));
#16714=DIRECTION('',(0.,0.,-1.));
#16715=DIRECTION('',(0.,0.,-1.));
#16716=DIRECTION('center_axis',(0.,0.,1.));
#16717=DIRECTION('ref_axis',(1.,0.,0.));
#16718=DIRECTION('center_axis',(0.,0.,1.));
#16719=DIRECTION('ref_axis',(1.,0.,0.));
#16720=DIRECTION('center_axis',(0.,0.,1.));
#16721=DIRECTION('ref_axis',(1.,0.,0.));
#16722=DIRECTION('axis',(0.,0.,1.));
#16723=DIRECTION('refdir',(1.,0.,0.));
#16724=DIRECTION('center_axis',(1.,0.,0.));
#16725=DIRECTION('ref_axis',(0.,0.,-1.));
#16726=DIRECTION('',(0.,0.,1.));
#16727=DIRECTION('center_axis',(1.,0.,0.));
#16728=DIRECTION('ref_axis',(0.,0.,-1.));
#16729=DIRECTION('center_axis',(1.,0.,0.));
#16730=DIRECTION('ref_axis',(0.,0.,-1.));
#16731=DIRECTION('center_axis',(1.,0.,0.));
#16732=DIRECTION('ref_axis',(0.,0.,-1.));
#16733=DIRECTION('',(1.,0.,0.));
#16734=DIRECTION('center_axis',(1.,0.,0.));
#16735=DIRECTION('ref_axis',(0.,0.,-1.));
#16736=DIRECTION('',(0.,0.,-1.));
#16737=DIRECTION('center_axis',(0.,0.,1.));
#16738=DIRECTION('ref_axis',(1.,0.,0.));
#16739=DIRECTION('center_axis',(0.,0.,1.));
#16740=DIRECTION('ref_axis',(1.,0.,0.));
#16741=DIRECTION('',(0.,0.,1.));
#16742=DIRECTION('center_axis',(0.,0.,-1.));
#16743=DIRECTION('ref_axis',(1.,0.,0.));
#16744=DIRECTION('center_axis',(0.,0.,1.));
#16745=DIRECTION('ref_axis',(1.,0.,0.));
#16746=DIRECTION('center_axis',(0.,0.,1.));
#16747=DIRECTION('ref_axis',(1.,0.,0.));
#16748=DIRECTION('',(0.,0.,-1.));
#16749=DIRECTION('center_axis',(0.,0.,-1.));
#16750=DIRECTION('ref_axis',(1.,0.,0.));
#16751=DIRECTION('center_axis',(0.,0.,1.));
#16752=DIRECTION('ref_axis',(1.,0.,0.));
#16753=DIRECTION('center_axis',(0.,0.,1.));
#16754=DIRECTION('ref_axis',(1.,0.,0.));
#16755=DIRECTION('center_axis',(0.,0.,1.));
#16756=DIRECTION('ref_axis',(1.,0.,0.));
#16757=DIRECTION('',(0.,0.,-1.));
#16758=DIRECTION('center_axis',(0.,0.,1.));
#16759=DIRECTION('ref_axis',(1.,0.,0.));
#16760=DIRECTION('center_axis',(0.,0.,1.));
#16761=DIRECTION('ref_axis',(1.,0.,0.));
#16762=DIRECTION('center_axis',(0.,0.,1.));
#16763=DIRECTION('ref_axis',(1.,0.,0.));
#16764=DIRECTION('axis',(0.,0.,1.));
#16765=DIRECTION('refdir',(1.,0.,0.));
#16766=DIRECTION('center_axis',(0.,0.,1.));
#16767=DIRECTION('ref_axis',(1.,0.,0.));
#16768=DIRECTION('center_axis',(0.,0.,1.));
#16769=DIRECTION('ref_axis',(1.,0.,0.));
#16770=DIRECTION('',(0.,0.,-1.));
#16771=DIRECTION('center_axis',(0.,0.,1.));
#16772=DIRECTION('ref_axis',(1.,0.,0.));
#16773=DIRECTION('center_axis',(0.,0.,1.));
#16774=DIRECTION('ref_axis',(1.,0.,0.));
#16775=DIRECTION('center_axis',(0.,0.,1.));
#16776=DIRECTION('ref_axis',(1.,0.,0.));
#16777=DIRECTION('axis',(0.,0.,1.));
#16778=DIRECTION('refdir',(1.,0.,0.));
#16779=DIRECTION('center_axis',(1.,0.,0.));
#16780=DIRECTION('ref_axis',(0.,0.,-1.));
#16781=DIRECTION('center_axis',(1.,0.,0.));
#16782=DIRECTION('ref_axis',(0.,0.,-1.));
#16783=DIRECTION('',(-1.,0.,0.));
#16784=DIRECTION('center_axis',(1.,0.,0.));
#16785=DIRECTION('ref_axis',(0.,0.,-1.));
#16786=DIRECTION('center_axis',(1.,0.,0.));
#16787=DIRECTION('ref_axis',(0.,0.,-1.));
#16788=DIRECTION('center_axis',(1.,0.,0.));
#16789=DIRECTION('ref_axis',(0.,0.,-1.));
#16790=DIRECTION('axis',(0.,0.,1.));
#16791=DIRECTION('refdir',(1.,0.,0.));
#16792=DIRECTION('center_axis',(1.,0.,0.));
#16793=DIRECTION('ref_axis',(0.,0.,-1.));
#16794=DIRECTION('',(1.,0.,0.));
#16795=DIRECTION('center_axis',(0.,1.,0.));
#16796=DIRECTION('ref_axis',(-1.,0.,0.));
#16797=DIRECTION('',(-1.,0.,0.));
#16798=DIRECTION('',(0.,0.,1.));
#16799=DIRECTION('',(1.,0.,0.));
#16800=DIRECTION('',(0.,0.,1.));
#16801=DIRECTION('center_axis',(1.,0.,0.));
#16802=DIRECTION('ref_axis',(0.,1.,0.));
#16803=DIRECTION('',(0.,1.,0.));
#16804=DIRECTION('',(0.,0.,1.));
#16805=DIRECTION('',(0.,-1.,0.));
#16806=DIRECTION('',(0.,0.,1.));
#16807=DIRECTION('center_axis',(1.,0.,0.));
#16808=DIRECTION('ref_axis',(0.,1.,0.));
#16809=DIRECTION('',(0.,1.,0.));
#16810=DIRECTION('',(0.,0.,-1.));
#16811=DIRECTION('',(0.,-1.,0.));
#16812=DIRECTION('center_axis',(0.,-1.,0.));
#16813=DIRECTION('ref_axis',(1.,0.,0.));
#16814=DIRECTION('',(1.,0.,0.));
#16815=DIRECTION('',(0.,0.,-1.));
#16816=DIRECTION('',(-1.,0.,0.));
#16817=DIRECTION('center_axis',(0.,0.,1.));
#16818=DIRECTION('ref_axis',(1.,0.,0.));
#16819=DIRECTION('center_axis',(0.,0.,-1.));
#16820=DIRECTION('ref_axis',(1.,0.,0.));
#16821=DIRECTION('center_axis',(0.,0.,1.));
#16822=DIRECTION('ref_axis',(1.,0.,0.));
#16823=DIRECTION('center_axis',(0.,0.,1.));
#16824=DIRECTION('ref_axis',(1.,0.,0.));
#16825=DIRECTION('center_axis',(0.,0.,1.));
#16826=DIRECTION('ref_axis',(1.,0.,0.));
#16827=DIRECTION('center_axis',(0.,0.,1.));
#16828=DIRECTION('ref_axis',(1.,0.,0.));
#16829=DIRECTION('center_axis',(0.,0.,-1.));
#16830=DIRECTION('ref_axis',(1.,0.,0.));
#16831=DIRECTION('center_axis',(0.,0.,1.));
#16832=DIRECTION('ref_axis',(1.,0.,0.));
#16833=DIRECTION('axis',(0.,0.,1.));
#16834=DIRECTION('refdir',(1.,0.,0.));
#16835=DIRECTION('center_axis',(0.866025403784439,0.,-0.5));
#16836=DIRECTION('ref_axis',(0.5,0.,0.866025403784439));
#16837=DIRECTION('',(0.5,0.,0.866025403784439));
#16838=DIRECTION('',(0.,-1.,0.));
#16839=DIRECTION('',(0.5,0.,0.866025403784439));
#16840=DIRECTION('',(0.,-1.,0.));
#16841=DIRECTION('center_axis',(1.20185167898973E-16,0.,-1.));
#16842=DIRECTION('ref_axis',(1.,0.,1.20185167898973E-16));
#16843=DIRECTION('',(1.,0.,1.20185167898973E-16));
#16844=DIRECTION('',(0.,-1.,0.));
#16845=DIRECTION('',(1.,0.,1.20185167898973E-16));
#16846=DIRECTION('center_axis',(-0.866025403784439,0.,-0.5));
#16847=DIRECTION('ref_axis',(0.5,0.,-0.866025403784439));
#16848=DIRECTION('',(0.5,0.,-0.866025403784439));
#16849=DIRECTION('',(0.,-1.,0.));
#16850=DIRECTION('',(0.5,0.,-0.866025403784439));
#16851=DIRECTION('center_axis',(-0.866025403784439,0.,0.5));
#16852=DIRECTION('ref_axis',(-0.5,0.,-0.866025403784439));
#16853=DIRECTION('',(-0.5,0.,-0.866025403784439));
#16854=DIRECTION('',(0.,-1.,0.));
#16855=DIRECTION('',(-0.5,0.,-0.866025403784439));
#16856=DIRECTION('center_axis',(-2.40370335797945E-16,0.,1.));
#16857=DIRECTION('ref_axis',(-1.,0.,-2.40370335797945E-16));
#16858=DIRECTION('',(-1.,0.,-2.40370335797945E-16));
#16859=DIRECTION('',(0.,-1.,0.));
#16860=DIRECTION('',(-1.,0.,-2.40370335797945E-16));
#16861=DIRECTION('center_axis',(0.866025403784439,0.,0.5));
#16862=DIRECTION('ref_axis',(-0.5,0.,0.866025403784439));
#16863=DIRECTION('',(-0.5,0.,0.866025403784439));
#16864=DIRECTION('',(-0.5,0.,0.866025403784439));
#16865=DIRECTION('center_axis',(0.,-1.,0.));
#16866=DIRECTION('ref_axis',(0.,0.,-1.));
#16867=DIRECTION('center_axis',(0.,1.,0.));
#16868=DIRECTION('ref_axis',(0.,0.,1.));
#16869=DIRECTION('center_axis',(0.,-1.,0.));
#16870=DIRECTION('ref_axis',(1.,0.,0.));
#16871=DIRECTION('center_axis',(0.,-1.,0.));
#16872=DIRECTION('ref_axis',(1.,0.,0.));
#16873=DIRECTION('center_axis',(0.,-1.,0.));
#16874=DIRECTION('ref_axis',(1.,0.,0.));
#16875=DIRECTION('',(0.707106781186548,0.707106781186547,8.65956056235494E-17));
#16876=DIRECTION('center_axis',(0.,-1.,0.));
#16877=DIRECTION('ref_axis',(1.,0.,0.));
#16878=DIRECTION('center_axis',(0.,1.,0.));
#16879=DIRECTION('ref_axis',(1.,0.,0.));
#16880=DIRECTION('',(0.,1.,0.));
#16881=DIRECTION('center_axis',(0.,1.,0.));
#16882=DIRECTION('ref_axis',(1.,0.,0.));
#16883=DIRECTION('center_axis',(0.,-1.,0.));
#16884=DIRECTION('ref_axis',(1.,0.,0.));
#16885=DIRECTION('',(-0.707106781186548,0.707106781186547,-8.65956056235494E-17));
#16886=DIRECTION('center_axis',(0.,-1.,0.));
#16887=DIRECTION('ref_axis',(0.,0.,-1.));
#16888=DIRECTION('',(0.,0.,1.));
#16889=DIRECTION('',(1.,0.,0.));
#16890=DIRECTION('',(0.,0.,1.));
#16891=DIRECTION('',(1.,0.,0.));
#16892=DIRECTION('',(0.,0.,1.));
#16893=DIRECTION('',(1.,0.,0.));
#16894=DIRECTION('',(0.,0.,1.));
#16895=DIRECTION('',(1.,0.,0.));
#16896=DIRECTION('',(0.,0.,1.));
#16897=DIRECTION('',(1.,0.,0.));
#16898=DIRECTION('',(0.,0.,1.));
#16899=DIRECTION('',(2.22044604925031E-16,-1.,0.));
#16900=DIRECTION('axis',(0.,0.,1.));
#16901=DIRECTION('refdir',(1.,0.,0.));
#16902=DIRECTION('axis',(0.,0.,1.));
#16903=DIRECTION('refdir',(1.,0.,0.));
#16904=DIRECTION('center_axis',(0.,1.,0.));
#16905=DIRECTION('ref_axis',(1.,0.,0.));
#16906=DIRECTION('center_axis',(0.,1.,0.));
#16907=DIRECTION('ref_axis',(1.,0.,0.));
#16908=DIRECTION('',(0.,1.,0.));
#16909=DIRECTION('center_axis',(0.,-1.,0.));
#16910=DIRECTION('ref_axis',(1.,0.,0.));
#16911=DIRECTION('center_axis',(0.,1.,0.));
#16912=DIRECTION('ref_axis',(1.,0.,0.));
#16913=DIRECTION('center_axis',(0.,1.,0.));
#16914=DIRECTION('ref_axis',(1.,0.,0.));
#16915=DIRECTION('center_axis',(0.,1.,0.));
#16916=DIRECTION('ref_axis',(1.,0.,0.));
#16917=DIRECTION('',(0.,1.,0.));
#16918=DIRECTION('center_axis',(0.,1.,0.));
#16919=DIRECTION('ref_axis',(1.,0.,0.));
#16920=DIRECTION('center_axis',(0.,1.,0.));
#16921=DIRECTION('ref_axis',(1.,0.,0.));
#16922=DIRECTION('center_axis',(0.,0.,-1.));
#16923=DIRECTION('ref_axis',(-1.,0.,0.));
#16924=DIRECTION('',(0.,-1.,0.));
#16925=DIRECTION('',(-1.,0.,0.));
#16926=DIRECTION('',(0.,1.,0.));
#16927=DIRECTION('',(1.,0.,0.));
#16928=DIRECTION('center_axis',(0.,1.,0.));
#16929=DIRECTION('ref_axis',(1.,0.,0.));
#16930=DIRECTION('center_axis',(0.,-1.,0.));
#16931=DIRECTION('ref_axis',(1.,0.,0.));
#16932=DIRECTION('',(0.,0.,-1.));
#16933=DIRECTION('',(-1.,0.,0.));
#16934=DIRECTION('center_axis',(-1.,0.,0.));
#16935=DIRECTION('ref_axis',(0.,0.,1.));
#16936=DIRECTION('',(0.,0.,1.));
#16937=DIRECTION('',(0.,1.,0.));
#16938=DIRECTION('center_axis',(0.,0.,1.));
#16939=DIRECTION('ref_axis',(1.,0.,0.));
#16940=DIRECTION('',(0.,1.,0.));
#16941=DIRECTION('',(1.,0.,0.));
#16942=DIRECTION('center_axis',(0.,1.,0.));
#16943=DIRECTION('ref_axis',(0.,0.,1.));
#16944=DIRECTION('center_axis',(0.,1.,0.));
#16945=DIRECTION('ref_axis',(1.,0.,0.));
#16946=DIRECTION('center_axis',(0.,0.,-1.));
#16947=DIRECTION('ref_axis',(-1.,0.,0.));
#16948=DIRECTION('',(0.,-1.,0.));
#16949=DIRECTION('',(-1.,0.,0.));
#16950=DIRECTION('',(0.,1.,0.));
#16951=DIRECTION('',(1.,0.,0.));
#16952=DIRECTION('center_axis',(0.,1.,0.));
#16953=DIRECTION('ref_axis',(1.,0.,0.));
#16954=DIRECTION('center_axis',(0.,-1.,0.));
#16955=DIRECTION('ref_axis',(1.,0.,0.));
#16956=DIRECTION('',(0.,0.,-1.));
#16957=DIRECTION('',(-1.,0.,0.));
#16958=DIRECTION('center_axis',(-1.,0.,0.));
#16959=DIRECTION('ref_axis',(0.,0.,1.));
#16960=DIRECTION('',(0.,0.,1.));
#16961=DIRECTION('',(0.,1.,0.));
#16962=DIRECTION('center_axis',(0.,0.,1.));
#16963=DIRECTION('ref_axis',(1.,0.,0.));
#16964=DIRECTION('',(0.,1.,0.));
#16965=DIRECTION('',(1.,0.,0.));
#16966=DIRECTION('center_axis',(0.,1.,0.));
#16967=DIRECTION('ref_axis',(0.,0.,1.));
#16968=DIRECTION('center_axis',(0.,1.,0.));
#16969=DIRECTION('ref_axis',(1.,0.,0.));
#16970=DIRECTION('center_axis',(0.,1.,0.));
#16971=DIRECTION('ref_axis',(1.,0.,0.));
#16972=DIRECTION('center_axis',(0.,1.,0.));
#16973=DIRECTION('ref_axis',(1.,0.,0.));
#16974=DIRECTION('',(0.,-1.,0.));
#16975=DIRECTION('center_axis',(0.,1.,0.));
#16976=DIRECTION('ref_axis',(1.,0.,0.));
#16977=DIRECTION('center_axis',(0.,1.,0.));
#16978=DIRECTION('ref_axis',(1.,0.,0.));
#16979=DIRECTION('center_axis',(0.,1.,0.));
#16980=DIRECTION('ref_axis',(1.,0.,0.));
#16981=DIRECTION('axis',(0.,0.,1.));
#16982=DIRECTION('refdir',(1.,0.,0.));
#16983=DIRECTION('center_axis',(0.,1.,0.));
#16984=DIRECTION('ref_axis',(1.,0.,0.));
#16985=DIRECTION('center_axis',(0.,-1.,0.));
#16986=DIRECTION('ref_axis',(1.,0.,0.));
#16987=DIRECTION('',(0.,-1.,0.));
#16988=DIRECTION('center_axis',(0.,-1.,0.));
#16989=DIRECTION('ref_axis',(1.,0.,0.));
#16990=DIRECTION('center_axis',(0.,1.,0.));
#16991=DIRECTION('ref_axis',(1.,0.,0.));
#16992=DIRECTION('center_axis',(0.,1.,0.));
#16993=DIRECTION('ref_axis',(1.,0.,0.));
#16994=DIRECTION('',(0.,-1.,0.));
#16995=DIRECTION('center_axis',(0.,1.,0.));
#16996=DIRECTION('ref_axis',(1.,0.,0.));
#16997=DIRECTION('center_axis',(0.,1.,0.));
#16998=DIRECTION('ref_axis',(1.,0.,0.));
#16999=DIRECTION('center_axis',(0.,1.,0.));
#17000=DIRECTION('ref_axis',(1.,0.,0.));
#17001=DIRECTION('axis',(0.,0.,1.));
#17002=DIRECTION('refdir',(1.,0.,0.));
#17003=DIRECTION('center_axis',(0.,1.,0.));
#17004=DIRECTION('ref_axis',(1.,0.,0.));
#17005=DIRECTION('center_axis',(0.,-1.,0.));
#17006=DIRECTION('ref_axis',(1.,0.,0.));
#17007=DIRECTION('',(0.,-1.,0.));
#17008=DIRECTION('center_axis',(0.,-1.,0.));
#17009=DIRECTION('ref_axis',(1.,0.,0.));
#17010=DIRECTION('center_axis',(0.,1.,0.));
#17011=DIRECTION('ref_axis',(1.,0.,0.));
#17012=DIRECTION('center_axis',(0.,1.,0.));
#17013=DIRECTION('ref_axis',(1.,0.,0.));
#17014=DIRECTION('',(0.,-1.,0.));
#17015=DIRECTION('center_axis',(0.,1.,0.));
#17016=DIRECTION('ref_axis',(1.,0.,0.));
#17017=DIRECTION('center_axis',(0.,1.,0.));
#17018=DIRECTION('ref_axis',(1.,0.,0.));
#17019=DIRECTION('center_axis',(0.,1.,0.));
#17020=DIRECTION('ref_axis',(1.,0.,0.));
#17021=DIRECTION('axis',(0.,0.,1.));
#17022=DIRECTION('refdir',(1.,0.,0.));
#17023=DIRECTION('center_axis',(0.,1.,0.));
#17024=DIRECTION('ref_axis',(1.,0.,0.));
#17025=DIRECTION('center_axis',(0.,-1.,0.));
#17026=DIRECTION('ref_axis',(1.,0.,0.));
#17027=DIRECTION('',(0.,-1.,0.));
#17028=DIRECTION('center_axis',(0.,-1.,0.));
#17029=DIRECTION('ref_axis',(1.,0.,0.));
#17030=DIRECTION('center_axis',(0.,1.,0.));
#17031=DIRECTION('ref_axis',(1.,0.,0.));
#17032=DIRECTION('center_axis',(0.,1.,0.));
#17033=DIRECTION('ref_axis',(1.,0.,0.));
#17034=DIRECTION('',(0.,-1.,0.));
#17035=DIRECTION('center_axis',(0.,1.,0.));
#17036=DIRECTION('ref_axis',(1.,0.,0.));
#17037=DIRECTION('center_axis',(0.,1.,0.));
#17038=DIRECTION('ref_axis',(1.,0.,0.));
#17039=DIRECTION('center_axis',(0.,1.,0.));
#17040=DIRECTION('ref_axis',(1.,0.,0.));
#17041=DIRECTION('axis',(0.,0.,1.));
#17042=DIRECTION('refdir',(1.,0.,0.));
#17043=DIRECTION('center_axis',(0.,1.,0.));
#17044=DIRECTION('ref_axis',(1.,0.,0.));
#17045=DIRECTION('center_axis',(0.,-1.,0.));
#17046=DIRECTION('ref_axis',(1.,0.,0.));
#17047=DIRECTION('',(0.,-1.,0.));
#17048=DIRECTION('center_axis',(0.,-1.,0.));
#17049=DIRECTION('ref_axis',(1.,0.,0.));
#17050=DIRECTION('center_axis',(0.,1.,0.));
#17051=DIRECTION('ref_axis',(1.,0.,0.));
#17052=DIRECTION('center_axis',(0.,1.,0.));
#17053=DIRECTION('ref_axis',(1.,0.,0.));
#17054=DIRECTION('',(0.,-1.,0.));
#17055=DIRECTION('center_axis',(0.,1.,0.));
#17056=DIRECTION('ref_axis',(1.,0.,0.));
#17057=DIRECTION('center_axis',(0.,1.,0.));
#17058=DIRECTION('ref_axis',(1.,0.,0.));
#17059=DIRECTION('center_axis',(0.,1.,0.));
#17060=DIRECTION('ref_axis',(1.,0.,0.));
#17061=DIRECTION('axis',(0.,0.,1.));
#17062=DIRECTION('refdir',(1.,0.,0.));
#17063=DIRECTION('center_axis',(0.,1.,0.));
#17064=DIRECTION('ref_axis',(-1.,0.,0.));
#17065=DIRECTION('',(-1.,0.,0.));
#17066=DIRECTION('',(0.,0.,1.));
#17067=DIRECTION('',(-1.,0.,0.));
#17068=DIRECTION('',(0.,0.,1.));
#17069=DIRECTION('center_axis',(1.,0.,0.));
#17070=DIRECTION('ref_axis',(0.,1.,0.));
#17071=DIRECTION('',(0.,1.,0.));
#17072=DIRECTION('',(0.,1.,0.));
#17073=DIRECTION('',(0.,0.,1.));
#17074=DIRECTION('center_axis',(0.,-1.,0.));
#17075=DIRECTION('ref_axis',(1.,0.,0.));
#17076=DIRECTION('',(1.,0.,0.));
#17077=DIRECTION('',(1.,0.,0.));
#17078=DIRECTION('',(0.,0.,1.));
#17079=DIRECTION('center_axis',(-1.,0.,0.));
#17080=DIRECTION('ref_axis',(0.,-1.,0.));
#17081=DIRECTION('',(0.,-1.,0.));
#17082=DIRECTION('',(0.,-1.,0.));
#17083=DIRECTION('center_axis',(0.,0.,1.));
#17084=DIRECTION('ref_axis',(1.,0.,0.));
#17085=DIRECTION('center_axis',(0.,0.,1.));
#17086=DIRECTION('ref_axis',(1.,0.,0.));
#17087=DIRECTION('axis',(0.,0.,1.));
#17088=DIRECTION('refdir',(1.,0.,0.));
#17089=DIRECTION('center_axis',(0.,1.,0.));
#17090=DIRECTION('ref_axis',(-1.,0.,0.));
#17091=DIRECTION('',(-1.,0.,0.));
#17092=DIRECTION('',(0.,0.,1.));
#17093=DIRECTION('',(-1.,0.,0.));
#17094=DIRECTION('',(0.,0.,1.));
#17095=DIRECTION('center_axis',(1.,0.,0.));
#17096=DIRECTION('ref_axis',(0.,1.,0.));
#17097=DIRECTION('',(0.,1.,0.));
#17098=DIRECTION('',(0.,1.,0.));
#17099=DIRECTION('',(0.,0.,1.));
#17100=DIRECTION('center_axis',(0.,-1.,0.));
#17101=DIRECTION('ref_axis',(1.,0.,0.));
#17102=DIRECTION('',(1.,0.,0.));
#17103=DIRECTION('',(1.,0.,0.));
#17104=DIRECTION('',(0.,0.,1.));
#17105=DIRECTION('center_axis',(-1.,0.,0.));
#17106=DIRECTION('ref_axis',(0.,-1.,0.));
#17107=DIRECTION('',(0.,-1.,0.));
#17108=DIRECTION('',(0.,-1.,0.));
#17109=DIRECTION('center_axis',(0.,0.,1.));
#17110=DIRECTION('ref_axis',(1.,0.,0.));
#17111=DIRECTION('center_axis',(0.,0.,1.));
#17112=DIRECTION('ref_axis',(1.,0.,0.));
#17113=DIRECTION('axis',(0.,0.,1.));
#17114=DIRECTION('refdir',(1.,0.,0.));
#17115=DIRECTION('center_axis',(0.,1.,0.));
#17116=DIRECTION('ref_axis',(1.,0.,0.));
#17117=DIRECTION('center_axis',(0.,1.,0.));
#17118=DIRECTION('ref_axis',(1.,0.,0.));
#17119=DIRECTION('',(0.,1.,0.));
#17120=DIRECTION('center_axis',(0.,-1.,0.));
#17121=DIRECTION('ref_axis',(1.,0.,0.));
#17122=DIRECTION('center_axis',(0.,0.,-1.));
#17123=DIRECTION('ref_axis',(-1.,0.,0.));
#17124=DIRECTION('',(-1.,0.,0.));
#17125=DIRECTION('',(0.,1.,0.));
#17126=DIRECTION('',(1.,0.,0.));
#17127=DIRECTION('',(0.,1.,0.));
#17128=DIRECTION('center_axis',(1.,0.,0.));
#17129=DIRECTION('ref_axis',(0.,0.,-1.));
#17130=DIRECTION('',(0.,0.,-1.));
#17131=DIRECTION('',(0.,1.,0.));
#17132=DIRECTION('',(0.,0.,1.));
#17133=DIRECTION('center_axis',(0.,0.,1.));
#17134=DIRECTION('ref_axis',(1.,0.,0.));
#17135=DIRECTION('',(1.,0.,0.));
#17136=DIRECTION('',(0.,-1.,0.));
#17137=DIRECTION('',(-1.,0.,0.));
#17138=DIRECTION('center_axis',(0.,1.,0.));
#17139=DIRECTION('ref_axis',(1.,0.,0.));
#17140=DIRECTION('center_axis',(0.,1.,0.));
#17141=DIRECTION('ref_axis',(1.,0.,0.));
#17142=DIRECTION('center_axis',(0.,-1.,0.));
#17143=DIRECTION('ref_axis',(1.,0.,0.));
#17144=DIRECTION('center_axis',(0.,1.,0.));
#17145=DIRECTION('ref_axis',(-1.,0.,-1.22464679914735E-16));
#17146=DIRECTION('center_axis',(0.,-1.,0.));
#17147=DIRECTION('ref_axis',(1.,0.,0.));
#17148=DIRECTION('center_axis',(0.,1.,0.));
#17149=DIRECTION('ref_axis',(6.12323399573677E-17,0.,1.));
#17150=DIRECTION('',(0.,-1.,0.));
#17151=DIRECTION('center_axis',(0.,1.,0.));
#17152=DIRECTION('ref_axis',(1.,0.,0.));
#17153=DIRECTION('',(0.,1.,0.));
#17154=DIRECTION('center_axis',(0.,1.,0.));
#17155=DIRECTION('ref_axis',(1.,0.,0.));
#17156=DIRECTION('center_axis',(1.,0.,0.));
#17157=DIRECTION('ref_axis',(0.,0.,-1.));
#17158=DIRECTION('',(0.,0.,1.));
#17159=DIRECTION('',(0.,-1.,0.));
#17160=DIRECTION('',(0.,0.,-1.));
#17161=DIRECTION('center_axis',(0.,1.,0.));
#17162=DIRECTION('ref_axis',(1.,0.,0.));
#17163=DIRECTION('',(0.,0.,-1.));
#17164=DIRECTION('center_axis',(0.,-1.,0.));
#17165=DIRECTION('ref_axis',(1.,0.,0.));
#17166=DIRECTION('center_axis',(-1.,0.,0.));
#17167=DIRECTION('ref_axis',(0.,0.,1.));
#17168=DIRECTION('',(0.,0.,1.));
#17169=DIRECTION('',(0.,1.,0.));
#17170=DIRECTION('center_axis',(0.,1.,0.));
#17171=DIRECTION('ref_axis',(0.,0.,1.));
#17172=DIRECTION('center_axis',(0.,1.,0.));
#17173=DIRECTION('ref_axis',(1.,0.,0.));
#17174=DIRECTION('center_axis',(0.,1.,0.));
#17175=DIRECTION('ref_axis',(1.,0.,0.));
#17176=DIRECTION('',(0.,-1.,0.));
#17177=DIRECTION('center_axis',(0.,1.,0.));
#17178=DIRECTION('ref_axis',(1.,0.,0.));
#17179=DIRECTION('center_axis',(0.,1.,0.));
#17180=DIRECTION('ref_axis',(1.,0.,0.));
#17181=DIRECTION('axis',(0.,0.,1.));
#17182=DIRECTION('refdir',(1.,0.,0.));
#17183=DIRECTION('center_axis',(0.,1.,0.));
#17184=DIRECTION('ref_axis',(1.,0.,0.));
#17185=DIRECTION('center_axis',(0.,-1.,0.));
#17186=DIRECTION('ref_axis',(1.,0.,0.));
#17187=DIRECTION('',(0.,-1.,0.));
#17188=DIRECTION('center_axis',(0.,-1.,0.));
#17189=DIRECTION('ref_axis',(1.,0.,0.));
#17190=DIRECTION('center_axis',(0.,1.,0.));
#17191=DIRECTION('ref_axis',(1.,0.,0.));
#17192=DIRECTION('center_axis',(0.,1.,0.));
#17193=DIRECTION('ref_axis',(1.,0.,0.));
#17194=DIRECTION('',(0.,-1.,0.));
#17195=DIRECTION('center_axis',(0.,1.,0.));
#17196=DIRECTION('ref_axis',(1.,0.,0.));
#17197=DIRECTION('center_axis',(0.,1.,0.));
#17198=DIRECTION('ref_axis',(1.,0.,0.));
#17199=DIRECTION('center_axis',(0.,1.,0.));
#17200=DIRECTION('ref_axis',(1.,0.,0.));
#17201=DIRECTION('axis',(0.,0.,1.));
#17202=DIRECTION('refdir',(1.,0.,0.));
#17203=DIRECTION('center_axis',(0.,1.,0.));
#17204=DIRECTION('ref_axis',(1.,0.,0.));
#17205=DIRECTION('center_axis',(0.,-1.,0.));
#17206=DIRECTION('ref_axis',(1.,0.,0.));
#17207=DIRECTION('',(0.,-1.,0.));
#17208=DIRECTION('center_axis',(0.,-1.,0.));
#17209=DIRECTION('ref_axis',(1.,0.,0.));
#17210=DIRECTION('center_axis',(0.,1.,0.));
#17211=DIRECTION('ref_axis',(1.,0.,0.));
#17212=DIRECTION('center_axis',(0.,1.,0.));
#17213=DIRECTION('ref_axis',(1.,0.,0.));
#17214=DIRECTION('',(0.,-1.,0.));
#17215=DIRECTION('center_axis',(0.,1.,0.));
#17216=DIRECTION('ref_axis',(1.,0.,0.));
#17217=DIRECTION('center_axis',(0.,1.,0.));
#17218=DIRECTION('ref_axis',(1.,0.,0.));
#17219=DIRECTION('center_axis',(0.,1.,0.));
#17220=DIRECTION('ref_axis',(1.,0.,0.));
#17221=DIRECTION('axis',(0.,0.,1.));
#17222=DIRECTION('refdir',(1.,0.,0.));
#17223=DIRECTION('center_axis',(0.,1.,0.));
#17224=DIRECTION('ref_axis',(1.,0.,0.));
#17225=DIRECTION('center_axis',(0.,-1.,0.));
#17226=DIRECTION('ref_axis',(1.,0.,0.));
#17227=DIRECTION('',(0.,-1.,0.));
#17228=DIRECTION('center_axis',(0.,-1.,0.));
#17229=DIRECTION('ref_axis',(1.,0.,0.));
#17230=DIRECTION('center_axis',(0.,1.,0.));
#17231=DIRECTION('ref_axis',(1.,0.,0.));
#17232=DIRECTION('center_axis',(0.,1.,0.));
#17233=DIRECTION('ref_axis',(1.,0.,0.));
#17234=DIRECTION('',(0.,-1.,0.));
#17235=DIRECTION('center_axis',(0.,1.,0.));
#17236=DIRECTION('ref_axis',(1.,0.,0.));
#17237=DIRECTION('center_axis',(0.,1.,0.));
#17238=DIRECTION('ref_axis',(1.,0.,0.));
#17239=DIRECTION('center_axis',(0.,1.,0.));
#17240=DIRECTION('ref_axis',(1.,0.,0.));
#17241=DIRECTION('axis',(0.,0.,1.));
#17242=DIRECTION('refdir',(1.,0.,0.));
#17243=DIRECTION('center_axis',(1.,0.,0.));
#17244=DIRECTION('ref_axis',(0.,0.,-1.));
#17245=DIRECTION('',(0.,0.,1.));
#17246=DIRECTION('',(0.,1.,0.));
#17247=DIRECTION('',(0.,0.,-1.));
#17248=DIRECTION('',(0.,-1.,0.));
#17249=DIRECTION('center_axis',(0.,0.,-1.));
#17250=DIRECTION('ref_axis',(-1.,0.,0.));
#17251=DIRECTION('',(1.,0.,0.));
#17252=DIRECTION('',(0.,-1.,0.));
#17253=DIRECTION('',(-1.,0.,0.));
#17254=DIRECTION('center_axis',(-1.,0.,0.));
#17255=DIRECTION('ref_axis',(0.,0.,1.));
#17256=DIRECTION('',(0.,0.,-1.));
#17257=DIRECTION('',(0.,1.,0.));
#17258=DIRECTION('',(0.,0.,1.));
#17259=DIRECTION('center_axis',(0.,1.,0.));
#17260=DIRECTION('ref_axis',(1.,0.,0.));
#17261=DIRECTION('center_axis',(0.,-1.,0.));
#17262=DIRECTION('ref_axis',(1.,0.,0.));
#17263=DIRECTION('',(-0.587785252292473,0.,0.809016994374947));
#17264=DIRECTION('center_axis',(0.,-1.,0.));
#17265=DIRECTION('ref_axis',(1.,0.,0.));
#17266=DIRECTION('',(-0.809016994374948,0.,0.587785252292473));
#17267=DIRECTION('center_axis',(0.,-1.,0.));
#17268=DIRECTION('ref_axis',(1.,0.,0.));
#17269=DIRECTION('',(-0.951056516295154,0.,0.309016994374947));
#17270=DIRECTION('center_axis',(0.,-1.,0.));
#17271=DIRECTION('ref_axis',(1.,0.,0.));
#17272=DIRECTION('',(-1.,0.,-1.83697019872103E-16));
#17273=DIRECTION('center_axis',(0.,-1.,0.));
#17274=DIRECTION('ref_axis',(1.,0.,0.));
#17275=DIRECTION('',(-0.951056516295154,0.,-0.309016994374948));
#17276=DIRECTION('center_axis',(0.,-1.,0.));
#17277=DIRECTION('ref_axis',(1.,0.,0.));
#17278=DIRECTION('',(-0.809016994374947,0.,-0.587785252292473));
#17279=DIRECTION('center_axis',(0.,-1.,0.));
#17280=DIRECTION('ref_axis',(1.,0.,0.));
#17281=DIRECTION('',(-0.587785252292473,0.,-0.809016994374948));
#17282=DIRECTION('center_axis',(0.,-1.,0.));
#17283=DIRECTION('ref_axis',(1.,0.,0.));
#17284=DIRECTION('',(-0.309016994374947,0.,-0.951056516295154));
#17285=DIRECTION('center_axis',(0.,-1.,0.));
#17286=DIRECTION('ref_axis',(1.,0.,0.));
#17287=DIRECTION('',(1.22464679914735E-16,0.,-1.));
#17288=DIRECTION('center_axis',(0.,-1.,0.));
#17289=DIRECTION('ref_axis',(1.,0.,0.));
#17290=DIRECTION('',(0.309016994374948,0.,-0.951056516295154));
#17291=DIRECTION('center_axis',(0.,-1.,0.));
#17292=DIRECTION('ref_axis',(1.,0.,0.));
#17293=DIRECTION('',(0.587785252292473,0.,-0.809016994374947));
#17294=DIRECTION('center_axis',(0.,-1.,0.));
#17295=DIRECTION('ref_axis',(1.,0.,0.));
#17296=DIRECTION('',(0.809016994374948,0.,-0.587785252292473));
#17297=DIRECTION('center_axis',(0.,-1.,0.));
#17298=DIRECTION('ref_axis',(1.,0.,0.));
#17299=DIRECTION('',(0.951056516295154,0.,-0.309016994374947));
#17300=DIRECTION('center_axis',(0.,-1.,0.));
#17301=DIRECTION('ref_axis',(1.,0.,0.));
#17302=DIRECTION('',(1.,0.,6.12323399573677E-17));
#17303=DIRECTION('center_axis',(0.,-1.,0.));
#17304=DIRECTION('ref_axis',(1.,0.,0.));
#17305=DIRECTION('',(0.951056516295154,0.,0.309016994374948));
#17306=DIRECTION('center_axis',(0.,-1.,0.));
#17307=DIRECTION('ref_axis',(1.,0.,0.));
#17308=DIRECTION('',(0.809016994374947,0.,0.587785252292473));
#17309=DIRECTION('center_axis',(0.,-1.,0.));
#17310=DIRECTION('ref_axis',(1.,0.,0.));
#17311=DIRECTION('',(0.587785252292473,0.,0.809016994374947));
#17312=DIRECTION('center_axis',(0.,-1.,0.));
#17313=DIRECTION('ref_axis',(1.,0.,0.));
#17314=DIRECTION('',(0.309016994374947,0.,0.951056516295154));
#17315=DIRECTION('center_axis',(0.,-1.,0.));
#17316=DIRECTION('ref_axis',(1.,0.,0.));
#17317=DIRECTION('',(0.,0.,1.));
#17318=DIRECTION('center_axis',(0.,-1.,0.));
#17319=DIRECTION('ref_axis',(1.,0.,0.));
#17320=DIRECTION('',(-0.309016994374948,0.,0.951056516295154));
#17321=DIRECTION('center_axis',(0.,1.,0.));
#17322=DIRECTION('ref_axis',(1.,0.,0.));
#17323=DIRECTION('center_axis',(0.,1.,0.));
#17324=DIRECTION('ref_axis',(6.12323399573677E-17,0.,1.));
#17325=DIRECTION('center_axis',(0.,-1.,0.));
#17326=DIRECTION('ref_axis',(1.,0.,0.));
#17327=DIRECTION('center_axis',(0.,1.,0.));
#17328=DIRECTION('ref_axis',(1.,0.,0.));
#17329=DIRECTION('center_axis',(0.,1.,0.));
#17330=DIRECTION('ref_axis',(1.,0.,0.));
#17331=DIRECTION('',(0.,-1.,0.));
#17332=DIRECTION('center_axis',(0.,-1.,0.));
#17333=DIRECTION('ref_axis',(1.,0.,0.));
#17334=DIRECTION('center_axis',(0.,1.,0.));
#17335=DIRECTION('ref_axis',(1.,0.,0.));
#17336=DIRECTION('',(0.,-1.,0.));
#17337=DIRECTION('',(0.,1.,0.));
#17338=DIRECTION('center_axis',(0.951056516295154,0.,0.309016994374948));
#17339=DIRECTION('ref_axis',(0.309016994374948,0.,-0.951056516295154));
#17340=DIRECTION('',(0.309016994374948,0.,-0.951056516295154));
#17341=DIRECTION('',(0.,1.,0.));
#17342=DIRECTION('',(0.,1.,0.));
#17343=DIRECTION('center_axis',(0.,1.,0.));
#17344=DIRECTION('ref_axis',(1.,0.,0.));
#17345=DIRECTION('center_axis',(0.,1.,0.));
#17346=DIRECTION('ref_axis',(1.,0.,0.));
#17347=DIRECTION('',(0.,-1.,0.));
#17348=DIRECTION('',(0.,1.,0.));
#17349=DIRECTION('center_axis',(0.809016994374947,0.,0.587785252292473));
#17350=DIRECTION('ref_axis',(0.587785252292473,0.,-0.809016994374947));
#17351=DIRECTION('',(0.587785252292473,0.,-0.809016994374947));
#17352=DIRECTION('',(0.,1.,0.));
#17353=DIRECTION('',(0.,1.,0.));
#17354=DIRECTION('center_axis',(0.,1.,0.));
#17355=DIRECTION('ref_axis',(1.,0.,0.));
#17356=DIRECTION('center_axis',(0.,1.,0.));
#17357=DIRECTION('ref_axis',(1.,0.,0.));
#17358=DIRECTION('',(0.,-1.,0.));
#17359=DIRECTION('',(0.,1.,0.));
#17360=DIRECTION('center_axis',(0.587785252292473,0.,0.809016994374948));
#17361=DIRECTION('ref_axis',(0.809016994374948,0.,-0.587785252292473));
#17362=DIRECTION('',(0.809016994374948,0.,-0.587785252292473));
#17363=DIRECTION('',(0.,1.,0.));
#17364=DIRECTION('',(0.,1.,0.));
#17365=DIRECTION('center_axis',(0.,1.,0.));
#17366=DIRECTION('ref_axis',(1.,0.,0.));
#17367=DIRECTION('center_axis',(0.,1.,0.));
#17368=DIRECTION('ref_axis',(1.,0.,0.));
#17369=DIRECTION('',(0.,-1.,0.));
#17370=DIRECTION('',(0.,1.,0.));
#17371=DIRECTION('center_axis',(0.309016994374947,0.,0.951056516295154));
#17372=DIRECTION('ref_axis',(0.951056516295154,0.,-0.309016994374947));
#17373=DIRECTION('',(0.951056516295154,0.,-0.309016994374947));
#17374=DIRECTION('',(0.,1.,0.));
#17375=DIRECTION('',(0.,1.,0.));
#17376=DIRECTION('center_axis',(0.,1.,0.));
#17377=DIRECTION('ref_axis',(1.,0.,0.));
#17378=DIRECTION('center_axis',(0.,1.,0.));
#17379=DIRECTION('ref_axis',(1.,0.,0.));
#17380=DIRECTION('',(0.,-1.,0.));
#17381=DIRECTION('',(0.,1.,0.));
#17382=DIRECTION('center_axis',(-1.83697019872103E-16,0.,1.));
#17383=DIRECTION('ref_axis',(1.,0.,1.83697019872103E-16));
#17384=DIRECTION('',(1.,0.,1.83697019872103E-16));
#17385=DIRECTION('',(0.,1.,0.));
#17386=DIRECTION('',(0.,1.,0.));
#17387=DIRECTION('center_axis',(0.,1.,0.));
#17388=DIRECTION('ref_axis',(1.,0.,0.));
#17389=DIRECTION('center_axis',(0.,1.,0.));
#17390=DIRECTION('ref_axis',(1.,0.,0.));
#17391=DIRECTION('',(0.,-1.,0.));
#17392=DIRECTION('',(0.,1.,0.));
#17393=DIRECTION('center_axis',(-0.309016994374948,0.,0.951056516295154));
#17394=DIRECTION('ref_axis',(0.951056516295154,0.,0.309016994374948));
#17395=DIRECTION('',(0.951056516295154,0.,0.309016994374948));
#17396=DIRECTION('',(0.,1.,0.));
#17397=DIRECTION('',(0.,1.,0.));
#17398=DIRECTION('center_axis',(0.,1.,0.));
#17399=DIRECTION('ref_axis',(1.,0.,0.));
#17400=DIRECTION('center_axis',(0.,1.,0.));
#17401=DIRECTION('ref_axis',(1.,0.,0.));
#17402=DIRECTION('',(0.,-1.,0.));
#17403=DIRECTION('',(0.,1.,0.));
#17404=DIRECTION('center_axis',(-0.587785252292473,0.,0.809016994374947));
#17405=DIRECTION('ref_axis',(0.809016994374947,0.,0.587785252292473));
#17406=DIRECTION('',(0.809016994374947,0.,0.587785252292473));
#17407=DIRECTION('',(0.,1.,0.));
#17408=DIRECTION('',(0.,1.,0.));
#17409=DIRECTION('center_axis',(0.,1.,0.));
#17410=DIRECTION('ref_axis',(1.,0.,0.));
#17411=DIRECTION('center_axis',(0.,1.,0.));
#17412=DIRECTION('ref_axis',(1.,0.,0.));
#17413=DIRECTION('',(0.,-1.,0.));
#17414=DIRECTION('',(0.,1.,0.));
#17415=DIRECTION('center_axis',(-0.809016994374948,0.,0.587785252292473));
#17416=DIRECTION('ref_axis',(0.587785252292473,0.,0.809016994374948));
#17417=DIRECTION('',(0.587785252292473,0.,0.809016994374948));
#17418=DIRECTION('',(0.,1.,0.));
#17419=DIRECTION('',(0.,1.,0.));
#17420=DIRECTION('center_axis',(0.,1.,0.));
#17421=DIRECTION('ref_axis',(1.,0.,0.));
#17422=DIRECTION('center_axis',(0.,1.,0.));
#17423=DIRECTION('ref_axis',(1.,0.,0.));
#17424=DIRECTION('',(0.,-1.,0.));
#17425=DIRECTION('',(0.,1.,0.));
#17426=DIRECTION('center_axis',(-0.951056516295154,0.,0.309016994374947));
#17427=DIRECTION('ref_axis',(0.309016994374947,0.,0.951056516295154));
#17428=DIRECTION('',(0.309016994374947,0.,0.951056516295154));
#17429=DIRECTION('',(0.,1.,0.));
#17430=DIRECTION('',(0.,1.,0.));
#17431=DIRECTION('center_axis',(0.,1.,0.));
#17432=DIRECTION('ref_axis',(1.,0.,0.));
#17433=DIRECTION('center_axis',(0.,1.,0.));
#17434=DIRECTION('ref_axis',(1.,0.,0.));
#17435=DIRECTION('',(0.,-1.,0.));
#17436=DIRECTION('',(0.,1.,0.));
#17437=DIRECTION('center_axis',(-1.,0.,-1.22464679914735E-16));
#17438=DIRECTION('ref_axis',(-1.22464679914735E-16,0.,1.));
#17439=DIRECTION('',(-1.22464679914735E-16,0.,1.));
#17440=DIRECTION('',(0.,1.,0.));
#17441=DIRECTION('',(0.,1.,0.));
#17442=DIRECTION('center_axis',(0.,1.,0.));
#17443=DIRECTION('ref_axis',(1.,0.,0.));
#17444=DIRECTION('center_axis',(0.,1.,0.));
#17445=DIRECTION('ref_axis',(1.,0.,0.));
#17446=DIRECTION('',(0.,-1.,0.));
#17447=DIRECTION('',(0.,1.,0.));
#17448=DIRECTION('center_axis',(-0.951056516295154,0.,-0.309016994374948));
#17449=DIRECTION('ref_axis',(-0.309016994374948,0.,0.951056516295154));
#17450=DIRECTION('',(-0.309016994374948,0.,0.951056516295154));
#17451=DIRECTION('',(0.,1.,0.));
#17452=DIRECTION('',(0.,1.,0.));
#17453=DIRECTION('center_axis',(0.,1.,0.));
#17454=DIRECTION('ref_axis',(1.,0.,0.));
#17455=DIRECTION('center_axis',(0.,1.,0.));
#17456=DIRECTION('ref_axis',(1.,0.,0.));
#17457=DIRECTION('',(0.,-1.,0.));
#17458=DIRECTION('',(0.,1.,0.));
#17459=DIRECTION('center_axis',(-0.809016994374947,0.,-0.587785252292473));
#17460=DIRECTION('ref_axis',(-0.587785252292473,0.,0.809016994374947));
#17461=DIRECTION('',(-0.587785252292473,0.,0.809016994374947));
#17462=DIRECTION('',(0.,1.,0.));
#17463=DIRECTION('',(0.,1.,0.));
#17464=DIRECTION('center_axis',(0.,1.,0.));
#17465=DIRECTION('ref_axis',(1.,0.,0.));
#17466=DIRECTION('center_axis',(0.,1.,0.));
#17467=DIRECTION('ref_axis',(1.,0.,0.));
#17468=DIRECTION('',(0.,-1.,0.));
#17469=DIRECTION('',(0.,1.,0.));
#17470=DIRECTION('center_axis',(-0.587785252292473,0.,-0.809016994374948));
#17471=DIRECTION('ref_axis',(-0.809016994374948,0.,0.587785252292473));
#17472=DIRECTION('',(-0.809016994374948,0.,0.587785252292473));
#17473=DIRECTION('',(0.,1.,0.));
#17474=DIRECTION('',(0.,1.,0.));
#17475=DIRECTION('center_axis',(0.,1.,0.));
#17476=DIRECTION('ref_axis',(1.,0.,0.));
#17477=DIRECTION('center_axis',(0.,1.,0.));
#17478=DIRECTION('ref_axis',(1.,0.,0.));
#17479=DIRECTION('',(0.,-1.,0.));
#17480=DIRECTION('',(0.,1.,0.));
#17481=DIRECTION('center_axis',(-0.309016994374947,0.,-0.951056516295154));
#17482=DIRECTION('ref_axis',(-0.951056516295154,0.,0.309016994374947));
#17483=DIRECTION('',(-0.951056516295154,0.,0.309016994374947));
#17484=DIRECTION('',(0.,1.,0.));
#17485=DIRECTION('',(0.,1.,0.));
#17486=DIRECTION('center_axis',(0.,1.,0.));
#17487=DIRECTION('ref_axis',(1.,0.,0.));
#17488=DIRECTION('center_axis',(0.,1.,0.));
#17489=DIRECTION('ref_axis',(1.,0.,0.));
#17490=DIRECTION('',(0.,-1.,0.));
#17491=DIRECTION('',(0.,1.,0.));
#17492=DIRECTION('center_axis',(6.12323399573677E-17,0.,-1.));
#17493=DIRECTION('ref_axis',(-1.,0.,-6.12323399573677E-17));
#17494=DIRECTION('',(-1.,0.,-6.12323399573677E-17));
#17495=DIRECTION('',(0.,1.,0.));
#17496=DIRECTION('',(0.,1.,0.));
#17497=DIRECTION('center_axis',(0.,1.,0.));
#17498=DIRECTION('ref_axis',(1.,0.,0.));
#17499=DIRECTION('center_axis',(0.,1.,0.));
#17500=DIRECTION('ref_axis',(1.,0.,0.));
#17501=DIRECTION('',(0.,-1.,0.));
#17502=DIRECTION('',(0.,1.,0.));
#17503=DIRECTION('center_axis',(0.309016994374948,0.,-0.951056516295154));
#17504=DIRECTION('ref_axis',(-0.951056516295154,0.,-0.309016994374948));
#17505=DIRECTION('',(-0.951056516295154,0.,-0.309016994374948));
#17506=DIRECTION('',(0.,1.,0.));
#17507=DIRECTION('',(0.,1.,0.));
#17508=DIRECTION('center_axis',(0.,1.,0.));
#17509=DIRECTION('ref_axis',(1.,0.,0.));
#17510=DIRECTION('center_axis',(0.,1.,0.));
#17511=DIRECTION('ref_axis',(1.,0.,0.));
#17512=DIRECTION('',(0.,-1.,0.));
#17513=DIRECTION('',(0.,1.,0.));
#17514=DIRECTION('center_axis',(0.587785252292473,0.,-0.809016994374947));
#17515=DIRECTION('ref_axis',(-0.809016994374947,0.,-0.587785252292473));
#17516=DIRECTION('',(-0.809016994374947,0.,-0.587785252292473));
#17517=DIRECTION('',(0.,1.,0.));
#17518=DIRECTION('',(0.,1.,0.));
#17519=DIRECTION('center_axis',(0.,1.,0.));
#17520=DIRECTION('ref_axis',(1.,0.,0.));
#17521=DIRECTION('center_axis',(0.,1.,0.));
#17522=DIRECTION('ref_axis',(1.,0.,0.));
#17523=DIRECTION('',(0.,-1.,0.));
#17524=DIRECTION('',(0.,1.,0.));
#17525=DIRECTION('center_axis',(0.809016994374947,0.,-0.587785252292473));
#17526=DIRECTION('ref_axis',(-0.587785252292473,0.,-0.809016994374947));
#17527=DIRECTION('',(-0.587785252292473,0.,-0.809016994374947));
#17528=DIRECTION('',(0.,1.,0.));
#17529=DIRECTION('',(0.,1.,0.));
#17530=DIRECTION('center_axis',(0.,1.,0.));
#17531=DIRECTION('ref_axis',(1.,0.,0.));
#17532=DIRECTION('center_axis',(0.,1.,0.));
#17533=DIRECTION('ref_axis',(1.,0.,0.));
#17534=DIRECTION('',(0.,-1.,0.));
#17535=DIRECTION('',(0.,1.,0.));
#17536=DIRECTION('center_axis',(0.951056516295154,0.,-0.309016994374947));
#17537=DIRECTION('ref_axis',(-0.309016994374947,0.,-0.951056516295154));
#17538=DIRECTION('',(-0.309016994374947,0.,-0.951056516295154));
#17539=DIRECTION('',(0.,1.,0.));
#17540=DIRECTION('',(0.,1.,0.));
#17541=DIRECTION('center_axis',(0.,1.,0.));
#17542=DIRECTION('ref_axis',(1.,0.,0.));
#17543=DIRECTION('center_axis',(0.,1.,0.));
#17544=DIRECTION('ref_axis',(1.,0.,0.));
#17545=DIRECTION('',(0.,-1.,0.));
#17546=DIRECTION('',(0.,1.,0.));
#17547=DIRECTION('center_axis',(1.,0.,0.));
#17548=DIRECTION('ref_axis',(0.,0.,-1.));
#17549=DIRECTION('',(0.,0.,-1.));
#17550=DIRECTION('',(0.,1.,0.));
#17551=DIRECTION('',(0.,1.,0.));
#17552=DIRECTION('center_axis',(0.,1.,0.));
#17553=DIRECTION('ref_axis',(1.,0.,0.));
#17554=DIRECTION('center_axis',(0.,1.,0.));
#17555=DIRECTION('ref_axis',(1.,0.,0.));
#17556=DIRECTION('center_axis',(0.,1.,0.));
#17557=DIRECTION('ref_axis',(1.,0.,0.));
#17558=DIRECTION('axis',(0.,0.,1.));
#17559=DIRECTION('refdir',(1.,0.,0.));
#17560=DIRECTION('center_axis',(0.,1.,0.));
#17561=DIRECTION('ref_axis',(1.,0.,0.));
#17562=DIRECTION('center_axis',(0.,-1.,0.));
#17563=DIRECTION('ref_axis',(1.,0.,0.));
#17564=DIRECTION('',(0.,-1.,0.));
#17565=DIRECTION('center_axis',(0.,-1.,0.));
#17566=DIRECTION('ref_axis',(1.,0.,0.));
#17567=DIRECTION('center_axis',(0.,1.,0.));
#17568=DIRECTION('ref_axis',(1.,0.,0.));
#17569=DIRECTION('center_axis',(0.,1.,0.));
#17570=DIRECTION('ref_axis',(1.,0.,0.));
#17571=DIRECTION('',(0.,-1.,0.));
#17572=DIRECTION('center_axis',(0.,1.,0.));
#17573=DIRECTION('ref_axis',(1.,0.,0.));
#17574=DIRECTION('center_axis',(0.,1.,0.));
#17575=DIRECTION('ref_axis',(1.,0.,0.));
#17576=DIRECTION('center_axis',(0.,1.,0.));
#17577=DIRECTION('ref_axis',(1.,0.,0.));
#17578=DIRECTION('axis',(0.,0.,1.));
#17579=DIRECTION('refdir',(1.,0.,0.));
#17580=DIRECTION('center_axis',(0.,1.,0.));
#17581=DIRECTION('ref_axis',(0.,0.,1.));
#17582=DIRECTION('center_axis',(0.,-1.,0.));
#17583=DIRECTION('ref_axis',(1.,0.,0.));
#17584=DIRECTION('center_axis',(0.,-1.,0.));
#17585=DIRECTION('ref_axis',(1.,0.,0.));
#17586=DIRECTION('center_axis',(0.,-1.,0.));
#17587=DIRECTION('ref_axis',(1.,0.,0.));
#17588=DIRECTION('',(0.707106781186548,0.707106781186547,8.65956056235494E-17));
#17589=DIRECTION('center_axis',(0.,-1.,0.));
#17590=DIRECTION('ref_axis',(1.,0.,0.));
#17591=DIRECTION('center_axis',(0.,-1.,0.));
#17592=DIRECTION('ref_axis',(1.,0.,0.));
#17593=DIRECTION('',(0.,1.,0.));
#17594=DIRECTION('center_axis',(0.,1.,0.));
#17595=DIRECTION('ref_axis',(1.,0.,0.));
#17596=DIRECTION('center_axis',(0.,-1.,0.));
#17597=DIRECTION('ref_axis',(1.,0.,0.));
#17598=DIRECTION('',(-0.707106781186547,0.707106781186548,-8.65956056235493E-17));
#17599=DIRECTION('center_axis',(0.,-1.,0.));
#17600=DIRECTION('ref_axis',(0.,0.,-1.));
#17601=DIRECTION('center_axis',(0.,-1.,0.));
#17602=DIRECTION('ref_axis',(1.,0.,0.));
#17603=DIRECTION('center_axis',(0.,1.,0.));
#17604=DIRECTION('ref_axis',(1.,0.,0.));
#17605=DIRECTION('center_axis',(0.,1.,0.));
#17606=DIRECTION('ref_axis',(1.,0.,0.));
#17607=DIRECTION('',(-0.447213595499958,0.894427190999916,-5.47678698264203E-17));
#17608=DIRECTION('center_axis',(0.,-1.,0.));
#17609=DIRECTION('ref_axis',(1.,0.,0.));
#17610=DIRECTION('center_axis',(0.,1.,0.));
#17611=DIRECTION('ref_axis',(1.,0.,0.));
#17612=DIRECTION('',(0.,1.,0.));
#17613=DIRECTION('center_axis',(0.,1.,0.));
#17614=DIRECTION('ref_axis',(1.,0.,0.));
#17615=DIRECTION('center_axis',(0.,-1.,0.));
#17616=DIRECTION('ref_axis',(1.,0.,0.));
#17617=DIRECTION('',(-0.707106781186547,0.707106781186548,-8.65956056235493E-17));
#17618=DIRECTION('center_axis',(0.,-1.,0.));
#17619=DIRECTION('ref_axis',(0.,0.,-1.));
#17620=DIRECTION('center_axis',(0.866025403784439,0.,-0.5));
#17621=DIRECTION('ref_axis',(0.5,0.,0.866025403784439));
#17622=DIRECTION('',(-0.5,0.,-0.866025403784439));
#17623=DIRECTION('',(0.,-1.,0.));
#17624=DIRECTION('',(0.5,0.,0.866025403784439));
#17625=DIRECTION('',(0.,-1.,0.));
#17626=DIRECTION('center_axis',(1.92296268638356E-16,0.,-1.));
#17627=DIRECTION('ref_axis',(1.,0.,1.92296268638356E-16));
#17628=DIRECTION('',(-1.,0.,-1.92296268638356E-16));
#17629=DIRECTION('',(0.,-1.,0.));
#17630=DIRECTION('',(1.,0.,1.92296268638356E-16));
#17631=DIRECTION('center_axis',(-0.866025403784439,0.,-0.5));
#17632=DIRECTION('ref_axis',(0.5,0.,-0.866025403784439));
#17633=DIRECTION('',(-0.5,0.,0.866025403784438));
#17634=DIRECTION('',(0.,-1.,0.));
#17635=DIRECTION('',(0.5,0.,-0.866025403784438));
#17636=DIRECTION('center_axis',(-0.866025403784439,0.,0.5));
#17637=DIRECTION('ref_axis',(-0.5,0.,-0.866025403784439));
#17638=DIRECTION('',(0.5,0.,0.866025403784439));
#17639=DIRECTION('',(0.,-1.,0.));
#17640=DIRECTION('',(-0.5,0.,-0.866025403784439));
#17641=DIRECTION('center_axis',(-1.92296268638356E-16,0.,1.));
#17642=DIRECTION('ref_axis',(-1.,0.,-1.92296268638356E-16));
#17643=DIRECTION('',(1.,0.,1.92296268638356E-16));
#17644=DIRECTION('',(0.,-1.,0.));
#17645=DIRECTION('',(-1.,0.,-1.92296268638356E-16));
#17646=DIRECTION('center_axis',(0.866025403784439,0.,0.5));
#17647=DIRECTION('ref_axis',(-0.5,0.,0.866025403784439));
#17648=DIRECTION('',(0.5,0.,-0.866025403784439));
#17649=DIRECTION('',(-0.5,0.,0.866025403784439));
#17650=DIRECTION('center_axis',(0.,1.,0.));
#17651=DIRECTION('ref_axis',(1.,0.,0.));
#17652=DIRECTION('center_axis',(0.,-1.,0.));
#17653=DIRECTION('ref_axis',(0.,0.,-1.));
#17654=DIRECTION('axis',(0.,0.,1.));
#17655=DIRECTION('refdir',(1.,0.,0.));
#17656=DIRECTION('center_axis',(0.,1.,0.));
#17657=DIRECTION('ref_axis',(0.,0.,1.));
#17658=DIRECTION('center_axis',(0.,-1.,0.));
#17659=DIRECTION('ref_axis',(1.,0.,0.));
#17660=DIRECTION('center_axis',(0.,-1.,0.));
#17661=DIRECTION('ref_axis',(1.,0.,0.));
#17662=DIRECTION('center_axis',(0.,-1.,0.));
#17663=DIRECTION('ref_axis',(1.,0.,0.));
#17664=DIRECTION('',(0.707106781186547,0.707106781186548,8.65956056235493E-17));
#17665=DIRECTION('center_axis',(0.,-1.,0.));
#17666=DIRECTION('ref_axis',(1.,0.,0.));
#17667=DIRECTION('center_axis',(0.,-1.,0.));
#17668=DIRECTION('ref_axis',(1.,0.,0.));
#17669=DIRECTION('',(0.,1.,0.));
#17670=DIRECTION('center_axis',(0.,1.,0.));
#17671=DIRECTION('ref_axis',(1.,0.,0.));
#17672=DIRECTION('center_axis',(0.,-1.,0.));
#17673=DIRECTION('ref_axis',(1.,0.,0.));
#17674=DIRECTION('',(-0.707106781186547,0.707106781186548,-8.65956056235493E-17));
#17675=DIRECTION('center_axis',(0.,-1.,0.));
#17676=DIRECTION('ref_axis',(0.,0.,-1.));
#17677=DIRECTION('center_axis',(0.,-1.,0.));
#17678=DIRECTION('ref_axis',(1.,0.,0.));
#17679=DIRECTION('center_axis',(0.,1.,0.));
#17680=DIRECTION('ref_axis',(1.,0.,0.));
#17681=DIRECTION('center_axis',(0.,1.,0.));
#17682=DIRECTION('ref_axis',(1.,0.,0.));
#17683=DIRECTION('',(-0.447213595499958,0.894427190999916,-5.47678698264203E-17));
#17684=DIRECTION('center_axis',(0.,-1.,0.));
#17685=DIRECTION('ref_axis',(1.,0.,0.));
#17686=DIRECTION('center_axis',(0.,1.,0.));
#17687=DIRECTION('ref_axis',(1.,0.,0.));
#17688=DIRECTION('',(0.,1.,0.));
#17689=DIRECTION('center_axis',(0.,1.,0.));
#17690=DIRECTION('ref_axis',(1.,0.,0.));
#17691=DIRECTION('center_axis',(0.,-1.,0.));
#17692=DIRECTION('ref_axis',(1.,0.,0.));
#17693=DIRECTION('',(-0.707106781186547,0.707106781186548,-8.65956056235493E-17));
#17694=DIRECTION('center_axis',(0.,-1.,0.));
#17695=DIRECTION('ref_axis',(0.,0.,-1.));
#17696=DIRECTION('center_axis',(0.866025403784439,0.,-0.5));
#17697=DIRECTION('ref_axis',(0.5,0.,0.866025403784439));
#17698=DIRECTION('',(-0.5,0.,-0.866025403784439));
#17699=DIRECTION('',(0.,-1.,0.));
#17700=DIRECTION('',(0.5,0.,0.866025403784439));
#17701=DIRECTION('',(0.,-1.,0.));
#17702=DIRECTION('center_axis',(1.60246890531964E-16,0.,-1.));
#17703=DIRECTION('ref_axis',(1.,0.,1.60246890531964E-16));
#17704=DIRECTION('',(-1.,0.,-1.60246890531964E-16));
#17705=DIRECTION('',(0.,-1.,0.));
#17706=DIRECTION('',(1.,0.,1.60246890531964E-16));
#17707=DIRECTION('center_axis',(-0.866025403784439,0.,-0.5));
#17708=DIRECTION('ref_axis',(0.5,0.,-0.866025403784439));
#17709=DIRECTION('',(-0.5,0.,0.866025403784439));
#17710=DIRECTION('',(0.,-1.,0.));
#17711=DIRECTION('',(0.5,0.,-0.866025403784439));
#17712=DIRECTION('center_axis',(-0.866025403784439,0.,0.5));
#17713=DIRECTION('ref_axis',(-0.5,0.,-0.866025403784439));
#17714=DIRECTION('',(0.5,0.,0.866025403784439));
#17715=DIRECTION('',(0.,-1.,0.));
#17716=DIRECTION('',(-0.5,0.,-0.866025403784439));
#17717=DIRECTION('center_axis',(-1.60246890531964E-16,0.,1.));
#17718=DIRECTION('ref_axis',(-1.,0.,-1.60246890531964E-16));
#17719=DIRECTION('',(1.,0.,1.60246890531964E-16));
#17720=DIRECTION('',(0.,-1.,0.));
#17721=DIRECTION('',(-1.,0.,-1.60246890531964E-16));
#17722=DIRECTION('center_axis',(0.866025403784439,0.,0.5));
#17723=DIRECTION('ref_axis',(-0.5,0.,0.866025403784439));
#17724=DIRECTION('',(0.5,0.,-0.866025403784439));
#17725=DIRECTION('',(-0.5,0.,0.866025403784439));
#17726=DIRECTION('center_axis',(0.,1.,0.));
#17727=DIRECTION('ref_axis',(1.,0.,0.));
#17728=DIRECTION('center_axis',(0.,-1.,0.));
#17729=DIRECTION('ref_axis',(0.,0.,-1.));
#17730=DIRECTION('',(0.,0.,1.));
#17731=DIRECTION('',(1.,0.,0.));
#17732=DIRECTION('',(0.,0.,1.));
#17733=DIRECTION('',(1.,0.,0.));
#17734=DIRECTION('',(0.,0.,1.));
#17735=DIRECTION('',(1.,0.,0.));
#17736=DIRECTION('',(0.,0.,1.));
#17737=DIRECTION('',(1.,0.,0.));
#17738=DIRECTION('',(0.,0.,1.));
#17739=DIRECTION('',(1.,0.,0.));
#17740=DIRECTION('',(0.,0.,1.));
#17741=DIRECTION('',(1.,0.,0.));
#17742=DIRECTION('',(0.,0.,1.));
#17743=DIRECTION('',(1.,0.,0.));
#17744=DIRECTION('',(0.,0.,1.));
#17745=DIRECTION('',(1.,0.,0.));
#17746=DIRECTION('',(0.,0.,1.));
#17747=DIRECTION('',(1.,0.,0.));
#17748=DIRECTION('',(0.,0.,1.));
#17749=DIRECTION('',(1.,0.,0.));
#17750=DIRECTION('',(0.,0.,1.));
#17751=DIRECTION('',(1.,0.,0.));
#17752=DIRECTION('',(0.,0.,1.));
#17753=DIRECTION('',(1.,0.,0.));
#17754=DIRECTION('',(0.,0.,1.));
#17755=DIRECTION('',(1.,0.,0.));
#17756=DIRECTION('',(0.,0.,1.));
#17757=DIRECTION('',(1.,0.,0.));
#17758=DIRECTION('',(0.,0.,1.));
#17759=DIRECTION('',(1.,0.,0.));
#17760=DIRECTION('',(0.,0.,1.));
#17761=DIRECTION('',(1.,0.,0.));
#17762=DIRECTION('',(-1.,0.,2.22044604925031E-16));
#17763=DIRECTION('',(2.22044604925031E-16,0.,1.));
#17764=DIRECTION('',(0.,-1.,2.22044604925031E-16));
#17765=DIRECTION('',(1.,0.,0.));
#17766=DIRECTION('',(0.,-1.,2.22044604925031E-16));
#17767=DIRECTION('',(1.,0.,0.));
#17768=DIRECTION('',(0.,0.,1.));
#17769=DIRECTION('',(2.22044604925031E-16,-1.,0.));
#17770=DIRECTION('',(0.,0.,1.));
#17771=DIRECTION('',(2.22044604925031E-16,-1.,0.));
#17772=DIRECTION('',(0.,-1.,2.22044604925031E-16));
#17773=DIRECTION('',(1.,0.,0.));
#17774=DIRECTION('',(0.,-1.,2.22044604925031E-16));
#17775=DIRECTION('',(1.,0.,0.));
#17776=DIRECTION('',(0.,-1.,2.22044604925031E-16));
#17777=DIRECTION('',(1.,0.,0.));
#17778=DIRECTION('',(0.,-1.,2.22044604925031E-16));
#17779=DIRECTION('',(1.,0.,0.));
#17780=DIRECTION('',(0.,0.,1.));
#17781=DIRECTION('',(2.22044604925031E-16,-1.,0.));
#17782=DIRECTION('',(0.,-1.,2.22044604925031E-16));
#17783=DIRECTION('',(1.,0.,0.));
#17784=DIRECTION('',(0.,-1.,2.22044604925031E-16));
#17785=DIRECTION('',(1.,0.,0.));
#17786=DIRECTION('',(0.,0.,1.));
#17787=DIRECTION('',(1.,0.,0.));
#17788=DIRECTION('',(0.,0.,1.));
#17789=DIRECTION('',(-1.,1.22464679914735E-16,0.));
#17790=DIRECTION('',(0.,0.,1.));
#17791=DIRECTION('',(-1.,1.22464679914735E-16,0.));
#17792=DIRECTION('',(0.,0.,1.));
#17793=DIRECTION('',(-1.,1.22464679914735E-16,0.));
#17794=DIRECTION('',(0.,0.,1.));
#17795=DIRECTION('',(-1.,1.22464679914735E-16,0.));
#17796=DIRECTION('',(0.,0.,1.));
#17797=DIRECTION('',(1.,0.,0.));
#17798=DIRECTION('',(0.,0.,1.));
#17799=DIRECTION('',(1.,0.,0.));
#17800=DIRECTION('',(0.,0.,1.));
#17801=DIRECTION('',(1.,0.,0.));
#17802=DIRECTION('',(0.,0.,1.));
#17803=DIRECTION('',(1.,0.,0.));
#17804=DIRECTION('',(0.,-1.,2.22044604925031E-16));
#17805=DIRECTION('',(1.,0.,0.));
#17806=DIRECTION('',(0.,-1.,2.22044604925031E-16));
#17807=DIRECTION('',(1.,0.,0.));
#17808=DIRECTION('',(0.,0.,1.));
#17809=DIRECTION('',(1.,0.,0.));
#17810=DIRECTION('',(0.,0.,1.));
#17811=DIRECTION('',(-1.,1.22464679914735E-16,0.));
#17812=DIRECTION('',(0.,0.,1.));
#17813=DIRECTION('',(-1.,1.22464679914735E-16,0.));
#17814=DIRECTION('',(0.,0.,1.));
#17815=DIRECTION('',(-1.,1.22464679914735E-16,0.));
#17816=DIRECTION('',(0.,0.,1.));
#17817=DIRECTION('',(-1.,1.22464679914735E-16,0.));
#17818=DIRECTION('',(0.,0.,1.));
#17819=DIRECTION('',(1.,0.,0.));
#17820=DIRECTION('',(0.,0.,1.));
#17821=DIRECTION('',(1.,0.,0.));
#17822=DIRECTION('',(0.,0.,1.));
#17823=DIRECTION('',(1.,0.,0.));
#17824=DIRECTION('',(0.,0.,1.));
#17825=DIRECTION('',(1.,0.,0.));
#17826=DIRECTION('',(0.,0.,1.));
#17827=DIRECTION('',(1.,0.,0.));
#17828=DIRECTION('',(0.,0.,1.));
#17829=DIRECTION('',(1.,0.,0.));
#17830=DIRECTION('',(0.,0.,1.));
#17831=DIRECTION('',(1.,0.,0.));
#17832=DIRECTION('',(0.,0.,1.));
#17833=DIRECTION('',(1.,0.,0.));
#17834=DIRECTION('',(0.,0.,1.));
#17835=DIRECTION('',(1.,0.,0.));
#17836=DIRECTION('',(0.,0.,1.));
#17837=DIRECTION('',(1.,0.,0.));
#17838=DIRECTION('',(0.,0.,1.));
#17839=DIRECTION('',(1.,0.,0.));
#17840=DIRECTION('',(0.,0.,1.));
#17841=DIRECTION('',(1.,0.,0.));
#17842=DIRECTION('',(0.,0.,1.));
#17843=DIRECTION('',(1.,0.,0.));
#17844=DIRECTION('',(0.,0.,1.));
#17845=DIRECTION('',(1.,0.,0.));
#17846=DIRECTION('',(0.,0.,1.));
#17847=DIRECTION('',(1.,0.,0.));
#17848=DIRECTION('',(-1.,0.,2.22044604925031E-16));
#17849=DIRECTION('',(2.22044604925031E-16,0.,1.));
#17850=DIRECTION('',(0.,0.,1.));
#17851=DIRECTION('',(1.,0.,0.));
#17852=DIRECTION('',(0.,0.,1.));
#17853=DIRECTION('',(1.,0.,0.));
#17854=DIRECTION('',(0.,0.,1.));
#17855=DIRECTION('',(-1.,1.22464679914735E-16,0.));
#17856=DIRECTION('',(0.,0.,1.));
#17857=DIRECTION('',(1.,0.,0.));
#17858=DIRECTION('axis',(0.,0.,1.));
#17859=DIRECTION('refdir',(1.,0.,0.));
#17860=DIRECTION('axis',(0.,0.,1.));
#17861=DIRECTION('refdir',(1.,0.,0.));
#17862=DIRECTION('center_axis',(0.,1.,0.));
#17863=DIRECTION('ref_axis',(1.,0.,0.));
#17864=DIRECTION('center_axis',(0.,-1.,0.));
#17865=DIRECTION('ref_axis',(1.,0.,0.));
#17866=DIRECTION('',(0.,-1.,0.));
#17867=DIRECTION('center_axis',(0.,-1.,0.));
#17868=DIRECTION('ref_axis',(1.,0.,0.));
#17869=DIRECTION('center_axis',(0.,1.,0.));
#17870=DIRECTION('ref_axis',(1.,0.,0.));
#17871=DIRECTION('center_axis',(0.,1.,0.));
#17872=DIRECTION('ref_axis',(1.,0.,0.));
#17873=DIRECTION('',(0.,-1.,0.));
#17874=DIRECTION('center_axis',(0.,1.,0.));
#17875=DIRECTION('ref_axis',(1.,0.,0.));
#17876=DIRECTION('center_axis',(0.,1.,0.));
#17877=DIRECTION('ref_axis',(1.,0.,0.));
#17878=DIRECTION('center_axis',(0.,1.,0.));
#17879=DIRECTION('ref_axis',(1.,0.,0.));
#17880=DIRECTION('',(0.,0.,1.));
#17881=DIRECTION('',(1.,0.,0.));
#17882=DIRECTION('',(0.,0.,1.));
#17883=DIRECTION('',(1.,0.,0.));
#17884=DIRECTION('',(0.,0.,1.));
#17885=DIRECTION('',(1.,0.,0.));
#17886=DIRECTION('',(0.,0.,1.));
#17887=DIRECTION('',(1.,0.,0.));
#17888=DIRECTION('',(0.,0.,1.));
#17889=DIRECTION('',(1.,0.,0.));
#17890=CARTESIAN_POINT('',(0.,0.,0.));
#17891=CARTESIAN_POINT('',(0.,0.,0.));
#17892=CARTESIAN_POINT('',(0.,0.,0.));
#17893=CARTESIAN_POINT('Origin',(-6.05,3.,-0.1));
#17894=CARTESIAN_POINT('',(-6.215,3.,0.));
#17895=CARTESIAN_POINT('Origin',(-6.05,3.,0.));
#17896=CARTESIAN_POINT('',(-6.215,3.,1.));
#17897=CARTESIAN_POINT('',(-6.215,3.,-0.1));
#17898=CARTESIAN_POINT('Origin',(-6.05,3.,1.));
#17899=CARTESIAN_POINT('Origin',(-0.45,3.,-0.1));
#17900=CARTESIAN_POINT('',(-0.615,3.,0.));
#17901=CARTESIAN_POINT('Origin',(-0.45,3.,0.));
#17902=CARTESIAN_POINT('',(-0.615,3.,1.));
#17903=CARTESIAN_POINT('',(-0.615,3.,-0.1));
#17904=CARTESIAN_POINT('Origin',(-0.45,3.,1.));
#17905=CARTESIAN_POINT('Origin',(-6.05,-3.,-0.1));
#17906=CARTESIAN_POINT('',(-6.215,-3.,0.));
#17907=CARTESIAN_POINT('Origin',(-6.05,-3.,0.));
#17908=CARTESIAN_POINT('',(-6.215,-3.,1.));
#17909=CARTESIAN_POINT('',(-6.215,-3.,-0.1));
#17910=CARTESIAN_POINT('Origin',(-6.05,-3.,1.));
#17911=CARTESIAN_POINT('Origin',(-0.45,-3.,-0.1));
#17912=CARTESIAN_POINT('',(-0.615,-3.,0.));
#17913=CARTESIAN_POINT('Origin',(-0.45,-3.,0.));
#17914=CARTESIAN_POINT('',(-0.615,-3.,1.));
#17915=CARTESIAN_POINT('',(-0.615,-3.,-0.1));
#17916=CARTESIAN_POINT('Origin',(-0.45,-3.,1.));
#17917=CARTESIAN_POINT('Origin',(5.5,-1.6,-0.1));
#17918=CARTESIAN_POINT('',(5.335,-1.6,0.));
#17919=CARTESIAN_POINT('Origin',(5.5,-1.6,0.));
#17920=CARTESIAN_POINT('',(5.335,-1.6,1.));
#17921=CARTESIAN_POINT('',(5.335,-1.6,-0.1));
#17922=CARTESIAN_POINT('Origin',(5.5,-1.6,1.));
#17923=CARTESIAN_POINT('Origin',(5.5,1.6,-0.1));
#17924=CARTESIAN_POINT('',(5.335,1.6,0.));
#17925=CARTESIAN_POINT('Origin',(5.5,1.6,0.));
#17926=CARTESIAN_POINT('',(5.335,1.6,1.));
#17927=CARTESIAN_POINT('',(5.335,1.6,-0.1));
#17928=CARTESIAN_POINT('Origin',(5.5,1.6,1.));
#17929=CARTESIAN_POINT('Origin',(10.,9.,0.));
#17930=CARTESIAN_POINT('',(10.,9.,0.));
#17931=CARTESIAN_POINT('',(-8.,9.,0.));
#17932=CARTESIAN_POINT('',(10.,9.,0.));
#17933=CARTESIAN_POINT('',(-8.,9.,1.));
#17934=CARTESIAN_POINT('',(-8.,9.,0.));
#17935=CARTESIAN_POINT('',(10.,9.,1.));
#17936=CARTESIAN_POINT('',(10.,9.,1.));
#17937=CARTESIAN_POINT('',(10.,9.,0.));
#17938=CARTESIAN_POINT('Origin',(10.,-9.,0.));
#17939=CARTESIAN_POINT('',(10.,-9.,0.));
#17940=CARTESIAN_POINT('',(10.,-9.,0.));
#17941=CARTESIAN_POINT('',(10.,-9.,1.));
#17942=CARTESIAN_POINT('',(10.,-9.,1.));
#17943=CARTESIAN_POINT('',(10.,-9.,0.));
#17944=CARTESIAN_POINT('Origin',(-8.,-9.,0.));
#17945=CARTESIAN_POINT('',(-8.,-9.,0.));
#17946=CARTESIAN_POINT('',(-8.,-9.,0.));
#17947=CARTESIAN_POINT('',(-8.,-9.,1.));
#17948=CARTESIAN_POINT('',(-8.,-9.,1.));
#17949=CARTESIAN_POINT('',(-8.,-9.,0.));
#17950=CARTESIAN_POINT('Origin',(-8.,9.,0.));
#17951=CARTESIAN_POINT('',(-8.,9.,0.));
#17952=CARTESIAN_POINT('',(-8.,9.,1.));
#17953=CARTESIAN_POINT('Origin',(1.,0.,1.));
#17954=CARTESIAN_POINT('Origin',(1.,0.,0.));
#17955=CARTESIAN_POINT('',(0.,0.,0.));
#17956=CARTESIAN_POINT('Origin',(-7.,9.,-0.8));
#17957=CARTESIAN_POINT('',(-7.,9.,-0.8));
#17958=CARTESIAN_POINT('',(-8.,9.,-0.8));
#17959=CARTESIAN_POINT('',(-7.,9.,-0.8));
#17960=CARTESIAN_POINT('',(-8.,9.,0.));
#17961=CARTESIAN_POINT('',(-8.,9.,-0.8));
#17962=CARTESIAN_POINT('',(-7.,9.,0.));
#17963=CARTESIAN_POINT('',(-7.,9.,0.));
#17964=CARTESIAN_POINT('',(-7.,9.,-0.8));
#17965=CARTESIAN_POINT('Origin',(-7.,-9.,-0.8));
#17966=CARTESIAN_POINT('',(-7.,-9.,-0.8));
#17967=CARTESIAN_POINT('',(-7.,-9.,-0.8));
#17968=CARTESIAN_POINT('',(-7.,-9.,0.));
#17969=CARTESIAN_POINT('',(-7.,-9.,0.));
#17970=CARTESIAN_POINT('',(-7.,-9.,-0.8));
#17971=CARTESIAN_POINT('Origin',(-8.,-9.,-0.8));
#17972=CARTESIAN_POINT('',(-8.,-9.,-0.8));
#17973=CARTESIAN_POINT('',(-8.,-9.,-0.8));
#17974=CARTESIAN_POINT('',(-8.,-9.,0.));
#17975=CARTESIAN_POINT('',(-8.,-9.,0.));
#17976=CARTESIAN_POINT('',(-8.,-9.,-0.8));
#17977=CARTESIAN_POINT('Origin',(-8.,9.,-0.8));
#17978=CARTESIAN_POINT('',(-8.,9.,-0.8));
#17979=CARTESIAN_POINT('',(-8.,9.,0.));
#17980=CARTESIAN_POINT('Origin',(-7.5,0.,0.));
#17981=CARTESIAN_POINT('Origin',(-7.5,0.,-0.8));
#17982=CARTESIAN_POINT('',(0.,0.,0.));
#17983=CARTESIAN_POINT('Origin',(10.,9.,-0.8));
#17984=CARTESIAN_POINT('',(10.,9.,-0.8));
#17985=CARTESIAN_POINT('',(9.,9.,-0.8));
#17986=CARTESIAN_POINT('',(10.,9.,-0.8));
#17987=CARTESIAN_POINT('',(9.,9.,0.));
#17988=CARTESIAN_POINT('',(9.,9.,-0.8));
#17989=CARTESIAN_POINT('',(10.,9.,0.));
#17990=CARTESIAN_POINT('',(10.,9.,0.));
#17991=CARTESIAN_POINT('',(10.,9.,-0.8));
#17992=CARTESIAN_POINT('Origin',(10.,-9.,-0.8));
#17993=CARTESIAN_POINT('',(10.,-9.,-0.8));
#17994=CARTESIAN_POINT('',(10.,-9.,-0.8));
#17995=CARTESIAN_POINT('',(10.,-9.,0.));
#17996=CARTESIAN_POINT('',(10.,-9.,0.));
#17997=CARTESIAN_POINT('',(10.,-9.,-0.8));
#17998=CARTESIAN_POINT('Origin',(9.,-9.,-0.8));
#17999=CARTESIAN_POINT('',(9.,-9.,-0.8));
#18000=CARTESIAN_POINT('',(9.,-9.,-0.8));
#18001=CARTESIAN_POINT('',(9.,-9.,0.));
#18002=CARTESIAN_POINT('',(9.,-9.,0.));
#18003=CARTESIAN_POINT('',(9.,-9.,-0.8));
#18004=CARTESIAN_POINT('Origin',(9.,9.,-0.8));
#18005=CARTESIAN_POINT('',(9.,9.,-0.8));
#18006=CARTESIAN_POINT('',(9.,9.,0.));
#18007=CARTESIAN_POINT('Origin',(9.5,0.,0.));
#18008=CARTESIAN_POINT('Origin',(9.5,0.,-0.8));
#18009=CARTESIAN_POINT('',(0.,0.,0.));
#18010=CARTESIAN_POINT('Origin',(2.4,-1.6,24.4));
#18011=CARTESIAN_POINT('',(2.235,-1.6,24.4));
#18012=CARTESIAN_POINT('Origin',(2.4,-1.6,24.4));
#18013=CARTESIAN_POINT('',(2.235,-1.6,25.));
#18014=CARTESIAN_POINT('',(2.235,-1.6,24.4));
#18015=CARTESIAN_POINT('Origin',(2.4,-1.6,25.));
#18016=CARTESIAN_POINT('Origin',(2.4,-1.6,24.4));
#18017=CARTESIAN_POINT('Origin',(2.4,1.6,24.4));
#18018=CARTESIAN_POINT('',(2.235,1.6,24.4));
#18019=CARTESIAN_POINT('Origin',(2.4,1.6,24.4));
#18020=CARTESIAN_POINT('',(2.235,1.6,25.));
#18021=CARTESIAN_POINT('',(2.235,1.6,24.4));
#18022=CARTESIAN_POINT('Origin',(2.4,1.6,25.));
#18023=CARTESIAN_POINT('Origin',(2.4,1.6,24.4));
#18024=CARTESIAN_POINT('Origin',(0.21,1.01,22.9));
#18025=CARTESIAN_POINT('',(-0.726238685697896,1.01,23.));
#18026=CARTESIAN_POINT('',(-0.726238685697896,1.01,25.));
#18027=CARTESIAN_POINT('',(-0.726238685697896,1.01,23.));
#18028=CARTESIAN_POINT('',(0.0305156009506911,1.01,23.));
#18029=CARTESIAN_POINT('',(1.98,1.01,23.));
#18030=CARTESIAN_POINT('',(0.0305156009506911,1.01,25.));
#18031=CARTESIAN_POINT('',(0.0305156009506911,1.01,22.9));
#18032=CARTESIAN_POINT('',(1.98,1.01,25.));
#18033=CARTESIAN_POINT('Origin',(-1.1,-1.01,22.9));
#18034=CARTESIAN_POINT('',(-0.726238685697896,-1.01,25.));
#18035=CARTESIAN_POINT('',(-0.726238685697896,-1.01,23.));
#18036=CARTESIAN_POINT('',(-0.726238685697896,-1.01,23.));
#18037=CARTESIAN_POINT('',(0.0305156009506911,-1.01,25.));
#18038=CARTESIAN_POINT('',(1.325,-1.01,25.));
#18039=CARTESIAN_POINT('',(0.0305156009506911,-1.01,23.));
#18040=CARTESIAN_POINT('',(0.0305156009506911,-1.01,22.9));
#18041=CARTESIAN_POINT('',(1.325,-1.01,23.));
#18042=CARTESIAN_POINT('Origin',(3.75,0.,23.));
#18043=CARTESIAN_POINT('',(1.,2.,23.));
#18044=CARTESIAN_POINT('Origin',(1.,0.,23.));
#18045=CARTESIAN_POINT('',(4.5,2.,23.));
#18046=CARTESIAN_POINT('',(6.5,2.,23.));
#18047=CARTESIAN_POINT('',(4.5,-2.,23.));
#18048=CARTESIAN_POINT('',(4.5,1.25,23.));
#18049=CARTESIAN_POINT('',(1.,-2.,23.));
#18050=CARTESIAN_POINT('',(1.,-2.,23.));
#18051=CARTESIAN_POINT('Origin',(1.,0.,23.));
#18052=CARTESIAN_POINT('Origin',(1.,0.,23.));
#18053=CARTESIAN_POINT('Origin',(1.,0.,22.9));
#18054=CARTESIAN_POINT('Origin',(1.,0.,25.));
#18055=CARTESIAN_POINT('Origin',(1.,0.,23.));
#18056=CARTESIAN_POINT('',(1.,-2.,25.));
#18057=CARTESIAN_POINT('',(1.,-2.,23.));
#18058=CARTESIAN_POINT('Origin',(1.,0.,25.));
#18059=CARTESIAN_POINT('Origin',(1.,0.,23.));
#18060=CARTESIAN_POINT('',(1.,2.,25.));
#18061=CARTESIAN_POINT('Origin',(1.,0.,25.));
#18062=CARTESIAN_POINT('',(1.,2.,23.));
#18063=CARTESIAN_POINT('Origin',(3.75,0.,25.));
#18064=CARTESIAN_POINT('',(4.5,-2.,25.));
#18065=CARTESIAN_POINT('',(1.,-2.,25.));
#18066=CARTESIAN_POINT('',(4.5,2.,25.));
#18067=CARTESIAN_POINT('',(4.5,1.25,25.));
#18068=CARTESIAN_POINT('',(6.5,2.,25.));
#18069=CARTESIAN_POINT('Origin',(1.,-2.,23.));
#18070=CARTESIAN_POINT('',(4.5,-2.,18.));
#18071=CARTESIAN_POINT('Origin',(6.5,2.,23.));
#18072=CARTESIAN_POINT('',(4.5,2.,18.));
#18073=CARTESIAN_POINT('Origin',(2.4,-1.6,14.4));
#18074=CARTESIAN_POINT('',(2.235,-1.6,14.4));
#18075=CARTESIAN_POINT('Origin',(2.4,-1.6,14.4));
#18076=CARTESIAN_POINT('',(2.235,-1.6,15.));
#18077=CARTESIAN_POINT('',(2.235,-1.6,14.4));
#18078=CARTESIAN_POINT('Origin',(2.4,-1.6,15.));
#18079=CARTESIAN_POINT('Origin',(2.4,-1.6,14.4));
#18080=CARTESIAN_POINT('Origin',(2.4,1.6,14.4));
#18081=CARTESIAN_POINT('',(2.235,1.6,14.4));
#18082=CARTESIAN_POINT('Origin',(2.4,1.6,14.4));
#18083=CARTESIAN_POINT('',(2.235,1.6,15.));
#18084=CARTESIAN_POINT('',(2.235,1.6,14.4));
#18085=CARTESIAN_POINT('Origin',(2.4,1.6,15.));
#18086=CARTESIAN_POINT('Origin',(2.4,1.6,14.4));
#18087=CARTESIAN_POINT('Origin',(0.21,1.01,12.9));
#18088=CARTESIAN_POINT('',(-0.726238685697896,1.01,13.));
#18089=CARTESIAN_POINT('',(-0.726238685697896,1.01,15.));
#18090=CARTESIAN_POINT('',(-0.726238685697896,1.01,13.));
#18091=CARTESIAN_POINT('',(0.0305156009506911,1.01,13.));
#18092=CARTESIAN_POINT('',(2.855,1.01,13.));
#18093=CARTESIAN_POINT('',(0.0305156009506911,1.01,15.));
#18094=CARTESIAN_POINT('',(0.0305156009506911,1.01,12.9));
#18095=CARTESIAN_POINT('',(1.98,1.01,15.));
#18096=CARTESIAN_POINT('Origin',(-1.1,-1.01,12.9));
#18097=CARTESIAN_POINT('',(-0.726238685697896,-1.01,15.));
#18098=CARTESIAN_POINT('',(-0.726238685697896,-1.01,13.));
#18099=CARTESIAN_POINT('',(-0.726238685697896,-1.01,13.));
#18100=CARTESIAN_POINT('',(0.0305156009506911,-1.01,15.));
#18101=CARTESIAN_POINT('',(1.325,-1.01,15.));
#18102=CARTESIAN_POINT('',(0.0305156009506911,-1.01,13.));
#18103=CARTESIAN_POINT('',(0.0305156009506911,-1.01,12.9));
#18104=CARTESIAN_POINT('',(2.2,-1.01,13.));
#18105=CARTESIAN_POINT('Origin',(5.5,0.,13.));
#18106=CARTESIAN_POINT('',(1.,2.,13.));
#18107=CARTESIAN_POINT('Origin',(1.,0.,13.));
#18108=CARTESIAN_POINT('',(4.5,2.,13.));
#18109=CARTESIAN_POINT('',(6.5,2.,13.));
#18110=CARTESIAN_POINT('',(4.5,2.5,13.));
#18111=CARTESIAN_POINT('',(4.5,2.5,13.));
#18112=CARTESIAN_POINT('',(6.5,2.5,13.));
#18113=CARTESIAN_POINT('',(6.5,2.5,13.));
#18114=CARTESIAN_POINT('',(6.5,0.979795897113272,13.));
#18115=CARTESIAN_POINT('',(6.5,-2.5,13.));
#18116=CARTESIAN_POINT('',(4.1,-1.71450551880629E-16,13.));
#18117=CARTESIAN_POINT('Origin',(5.5,0.,13.));
#18118=CARTESIAN_POINT('',(6.5,-0.979795897113272,13.));
#18119=CARTESIAN_POINT('Origin',(5.5,0.,13.));
#18120=CARTESIAN_POINT('',(6.5,-2.5,13.));
#18121=CARTESIAN_POINT('',(6.5,-2.5,13.));
#18122=CARTESIAN_POINT('',(4.5,-2.5,13.));
#18123=CARTESIAN_POINT('',(4.5,-2.5,13.));
#18124=CARTESIAN_POINT('',(4.5,-2.,13.));
#18125=CARTESIAN_POINT('',(4.5,2.5,13.));
#18126=CARTESIAN_POINT('',(1.,-2.,13.));
#18127=CARTESIAN_POINT('',(1.,-2.,13.));
#18128=CARTESIAN_POINT('Origin',(1.,0.,13.));
#18129=CARTESIAN_POINT('Origin',(1.,0.,13.));
#18130=CARTESIAN_POINT('Origin',(1.,0.,12.9));
#18131=CARTESIAN_POINT('Origin',(1.,0.,15.));
#18132=CARTESIAN_POINT('Origin',(1.,0.,13.));
#18133=CARTESIAN_POINT('',(1.,-2.,15.));
#18134=CARTESIAN_POINT('',(1.,-2.,13.));
#18135=CARTESIAN_POINT('Origin',(1.,0.,15.));
#18136=CARTESIAN_POINT('Origin',(1.,0.,13.));
#18137=CARTESIAN_POINT('',(1.,2.,15.));
#18138=CARTESIAN_POINT('Origin',(1.,0.,15.));
#18139=CARTESIAN_POINT('',(1.,2.,13.));
#18140=CARTESIAN_POINT('Origin',(3.75,0.,15.));
#18141=CARTESIAN_POINT('',(4.5,-2.,15.));
#18142=CARTESIAN_POINT('',(1.,-2.,15.));
#18143=CARTESIAN_POINT('',(4.5,2.,15.));
#18144=CARTESIAN_POINT('',(4.5,1.25,15.));
#18145=CARTESIAN_POINT('',(6.5,2.,15.));
#18146=CARTESIAN_POINT('Origin',(6.5,2.,13.));
#18147=CARTESIAN_POINT('',(4.5,2.,13.));
#18148=CARTESIAN_POINT('Origin',(1.,-2.,13.));
#18149=CARTESIAN_POINT('',(4.5,-2.,13.));
#18150=CARTESIAN_POINT('Origin',(4.5,2.5,13.));
#18151=CARTESIAN_POINT('',(4.5,-2.5,31.));
#18152=CARTESIAN_POINT('',(4.5,-2.5,13.));
#18153=CARTESIAN_POINT('',(4.5,2.5,31.));
#18154=CARTESIAN_POINT('',(4.5,2.5,31.));
#18155=CARTESIAN_POINT('',(4.5,2.5,13.));
#18156=CARTESIAN_POINT('Origin',(6.09,0.,12.2));
#18157=CARTESIAN_POINT('',(6.09,0.133884278389961,12.1035634923901));
#18158=CARTESIAN_POINT('',(6.09,0.133884278389961,12.2964365076099));
#18159=CARTESIAN_POINT('',(6.09,0.133884278389961,11.5));
#18160=CARTESIAN_POINT('Origin',(6.09,0.,12.2));
#18161=CARTESIAN_POINT('Origin',(6.09,0.,12.2));
#18162=CARTESIAN_POINT('',(6.09,-0.133884278389961,12.1035634923901));
#18163=CARTESIAN_POINT('Ctrl Pts',(6.09,-0.133884278389961,12.1035634923901));
#18164=CARTESIAN_POINT('Ctrl Pts',(6.09119840340611,-0.128603165341394,
12.0962316423768));
#18165=CARTESIAN_POINT('Ctrl Pts',(6.09244064128815,-0.122792448979944,
12.0894472111884));
#18166=CARTESIAN_POINT('Ctrl Pts',(6.09651064111414,-0.10208383195986,12.0687385941683));
#18167=CARTESIAN_POINT('Ctrl Pts',(6.09954409498317,-0.0836002135946602,
12.0560565239921));
#18168=CARTESIAN_POINT('Ctrl Pts',(6.10381707438298,-0.0429774150042655,
12.0391843843662));
#18169=CARTESIAN_POINT('Ctrl Pts',(6.105,-0.0208299403327841,12.035));
#18170=CARTESIAN_POINT('Ctrl Pts',(6.105,0.020829940332784,12.035));
#18171=CARTESIAN_POINT('Ctrl Pts',(6.10381707438298,0.0429774150042655,
12.0391843843662));
#18172=CARTESIAN_POINT('Ctrl Pts',(6.09954409498317,0.0836002135946602,
12.0560565239921));
#18173=CARTESIAN_POINT('Ctrl Pts',(6.09651064111414,0.10208383195986,12.0687385941683));
#18174=CARTESIAN_POINT('Ctrl Pts',(6.09244064128815,0.122792448979943,12.0894472111884));
#18175=CARTESIAN_POINT('Ctrl Pts',(6.09119840340611,0.128603165341395,12.0962316423768));
#18176=CARTESIAN_POINT('Ctrl Pts',(6.09,0.133884278389961,12.1035634923901));
#18177=CARTESIAN_POINT('',(6.09,-0.133884278389961,12.2964365076099));
#18178=CARTESIAN_POINT('Origin',(6.09,0.,12.2));
#18179=CARTESIAN_POINT('',(6.105,-2.74505708527337E-17,12.365));
#18180=CARTESIAN_POINT('Ctrl Pts',(6.105,1.11022302462516E-16,12.365));
#18181=CARTESIAN_POINT('Ctrl Pts',(6.105,-0.0208299403327839,12.365));
#18182=CARTESIAN_POINT('Ctrl Pts',(6.10381707438298,-0.0429774150042655,
12.3608156156338));
#18183=CARTESIAN_POINT('Ctrl Pts',(6.09954409498317,-0.0836002135946602,
12.3439434760079));
#18184=CARTESIAN_POINT('Ctrl Pts',(6.09651064111414,-0.10208383195986,12.3312614058317));
#18185=CARTESIAN_POINT('Ctrl Pts',(6.09244064128815,-0.122792448979944,
12.3105527888116));
#18186=CARTESIAN_POINT('Ctrl Pts',(6.09119840340611,-0.128603165341395,
12.3037683576232));
#18187=CARTESIAN_POINT('Ctrl Pts',(6.09,-0.133884278389961,12.2964365076099));
#18188=CARTESIAN_POINT('',(6.9,-2.02066721859312E-17,12.365));
#18189=CARTESIAN_POINT('',(6.09,-2.02066721859312E-17,12.365));
#18190=CARTESIAN_POINT('',(6.8902427845524,0.164999999999999,12.2));
#18191=CARTESIAN_POINT('Ctrl Pts',(6.8902427845524,0.164999999999999,12.2));
#18192=CARTESIAN_POINT('Ctrl Pts',(6.8902427845524,0.164999999999999,12.17926146026));
#18193=CARTESIAN_POINT('Ctrl Pts',(6.89075468722975,0.160851447474559,12.1571538860416));
#18194=CARTESIAN_POINT('Ctrl Pts',(6.89259968365095,0.144006627864299,12.1165070705051));
#18195=CARTESIAN_POINT('Ctrl Pts',(6.89390570229761,0.131311408395221,12.0979661706037));
#18196=CARTESIAN_POINT('Ctrl Pts',(6.89635413416378,0.102033925885227,12.0686886880937));
#18197=CARTESIAN_POINT('Ctrl Pts',(6.89765618378145,0.0834929839417266,
12.0559933930893));
#18198=CARTESIAN_POINT('Ctrl Pts',(6.89949208802221,0.042846026446055,12.0391485178689));
#18199=CARTESIAN_POINT('Ctrl Pts',(6.9,0.0207384030457212,12.035));
#18200=CARTESIAN_POINT('Ctrl Pts',(6.9,-0.0207384030457212,12.035));
#18201=CARTESIAN_POINT('Ctrl Pts',(6.89949208802221,-0.0428460264460565,
12.0391485178689));
#18202=CARTESIAN_POINT('Ctrl Pts',(6.89765618378145,-0.0834929839417278,
12.0559933930893));
#18203=CARTESIAN_POINT('Ctrl Pts',(6.89635413416378,-0.102033925885227,
12.0686886880937));
#18204=CARTESIAN_POINT('Ctrl Pts',(6.89390570229761,-0.131311408395221,
12.0979661706037));
#18205=CARTESIAN_POINT('Ctrl Pts',(6.89259968365095,-0.144006627864299,
12.1165070705051));
#18206=CARTESIAN_POINT('Ctrl Pts',(6.89075468722975,-0.160851447474559,
12.1571538860416));
#18207=CARTESIAN_POINT('Ctrl Pts',(6.8902427845524,-0.164999999999999,12.17926146026));
#18208=CARTESIAN_POINT('Ctrl Pts',(6.8902427845524,-0.164999999999999,12.22073853974));
#18209=CARTESIAN_POINT('Ctrl Pts',(6.89075468722975,-0.160851447474559,
12.2428461139584));
#18210=CARTESIAN_POINT('Ctrl Pts',(6.89259968365095,-0.144006627864299,
12.2834929294949));
#18211=CARTESIAN_POINT('Ctrl Pts',(6.89390570229761,-0.131311408395221,
12.3020338293963));
#18212=CARTESIAN_POINT('Ctrl Pts',(6.89635413416378,-0.102033925885227,
12.3313113119063));
#18213=CARTESIAN_POINT('Ctrl Pts',(6.89765618378145,-0.0834929839417278,
12.3440066069107));
#18214=CARTESIAN_POINT('Ctrl Pts',(6.89949208802221,-0.0428460264460565,
12.3608514821311));
#18215=CARTESIAN_POINT('Ctrl Pts',(6.9,-0.0207384030457213,12.365));
#18216=CARTESIAN_POINT('Ctrl Pts',(6.9,-1.14491749414469E-16,12.365));
#18217=CARTESIAN_POINT('Ctrl Pts',(6.9,6.93889390390723E-17,12.365));
#18218=CARTESIAN_POINT('Ctrl Pts',(6.9,0.0207384030457213,12.365));
#18219=CARTESIAN_POINT('Ctrl Pts',(6.89949208802221,0.0428460264460564,
12.3608514821311));
#18220=CARTESIAN_POINT('Ctrl Pts',(6.89765618378145,0.0834929839417278,
12.3440066069107));
#18221=CARTESIAN_POINT('Ctrl Pts',(6.89635413416378,0.102033925885227,12.3313113119063));
#18222=CARTESIAN_POINT('Ctrl Pts',(6.89390570229761,0.131311408395221,12.3020338293963));
#18223=CARTESIAN_POINT('Ctrl Pts',(6.89259968365095,0.144006627864299,12.2834929294949));
#18224=CARTESIAN_POINT('Ctrl Pts',(6.89075468722975,0.160851447474559,12.2428461139584));
#18225=CARTESIAN_POINT('Ctrl Pts',(6.8902427845524,0.164999999999999,12.22073853974));
#18226=CARTESIAN_POINT('Ctrl Pts',(6.8902427845524,0.164999999999999,12.2));
#18227=CARTESIAN_POINT('Ctrl Pts',(6.09,0.133884278389961,12.2964365076099));
#18228=CARTESIAN_POINT('Ctrl Pts',(6.09119840340611,0.128603165341395,12.3037683576232));
#18229=CARTESIAN_POINT('Ctrl Pts',(6.09244064128815,0.122792448979944,12.3105527888116));
#18230=CARTESIAN_POINT('Ctrl Pts',(6.09651064111414,0.10208383195986,12.3312614058317));
#18231=CARTESIAN_POINT('Ctrl Pts',(6.09954409498317,0.0836002135946602,
12.3439434760079));
#18232=CARTESIAN_POINT('Ctrl Pts',(6.10381707438298,0.0429774150042655,
12.3608156156338));
#18233=CARTESIAN_POINT('Ctrl Pts',(6.105,0.0208299403327841,12.365));
#18234=CARTESIAN_POINT('Ctrl Pts',(6.105,6.93889390390723E-17,12.365));
#18235=CARTESIAN_POINT('Origin',(6.09,0.,12.2));
#18236=CARTESIAN_POINT('',(6.09,-0.133884278389961,11.5));
#18237=CARTESIAN_POINT('Origin',(5.5,0.,13.));
#18238=CARTESIAN_POINT('',(6.5,-2.5,13.));
#18239=CARTESIAN_POINT('Origin',(5.5,0.,13.));
#18240=CARTESIAN_POINT('Origin',(5.5,0.,11.5));
#18241=CARTESIAN_POINT('',(4.895,-7.40911313484149E-17,13.));
#18242=CARTESIAN_POINT('Origin',(5.5,0.,13.));
#18243=CARTESIAN_POINT('',(4.895,-7.40911313484149E-17,11.5));
#18244=CARTESIAN_POINT('',(4.895,-7.40911313484149E-17,11.5));
#18245=CARTESIAN_POINT('Origin',(5.5,0.,11.5));
#18246=CARTESIAN_POINT('Origin',(5.5,0.,11.5));
#18247=CARTESIAN_POINT('',(4.1,-1.71450551880629E-16,11.5));
#18248=CARTESIAN_POINT('',(4.1,-1.71450551880629E-16,11.5));
#18249=CARTESIAN_POINT('Origin',(5.5,0.,11.5));
#18250=CARTESIAN_POINT('Origin',(5.5,0.,11.5));
#18251=CARTESIAN_POINT('Origin',(6.5,2.5,13.));
#18252=CARTESIAN_POINT('',(6.5,2.5,31.));
#18253=CARTESIAN_POINT('',(6.5,2.5,31.));
#18254=CARTESIAN_POINT('',(6.5,2.5,13.));
#18255=CARTESIAN_POINT('Origin',(6.5,-2.5,13.));
#18256=CARTESIAN_POINT('',(6.5,-2.5,31.));
#18257=CARTESIAN_POINT('',(6.5,-2.5,31.));
#18258=CARTESIAN_POINT('',(6.5,-2.5,13.));
#18259=CARTESIAN_POINT('Origin',(4.5,-2.5,13.));
#18260=CARTESIAN_POINT('',(4.5,-2.5,31.));
#18261=CARTESIAN_POINT('Origin',(5.5,0.,31.));
#18262=CARTESIAN_POINT('Origin',(5.5,0.,13.));
#18263=CARTESIAN_POINT('',(0.,0.,0.));
#18264=CARTESIAN_POINT('Origin',(5.5,-1.6,1.5));
#18265=CARTESIAN_POINT('',(5.79505604098506,-1.3685546875,2.1));
#18266=CARTESIAN_POINT('',(5.79505604098506,-1.3685546875,1.5));
#18267=CARTESIAN_POINT('',(5.79505604098506,-1.3685546875,1.5));
#18268=CARTESIAN_POINT('',(5.20494395901494,-1.3685546875,2.1));
#18269=CARTESIAN_POINT('Origin',(5.5,-1.6,2.1));
#18270=CARTESIAN_POINT('',(5.20494395901494,-1.3685546875,1.5));
#18271=CARTESIAN_POINT('',(5.20494395901494,-1.3685546875,1.5));
#18272=CARTESIAN_POINT('Origin',(5.5,-1.6,1.5));
#18273=CARTESIAN_POINT('Origin',(5.5,-1.6,2.1));
#18274=CARTESIAN_POINT('Origin',(5.5,0.,2.1));
#18275=CARTESIAN_POINT('Origin',(5.5,1.6,1.5));
#18276=CARTESIAN_POINT('',(5.20494395901494,1.3685546875,2.1));
#18277=CARTESIAN_POINT('',(5.20494395901494,1.3685546875,1.5));
#18278=CARTESIAN_POINT('',(5.20494395901494,1.3685546875,1.5));
#18279=CARTESIAN_POINT('',(5.79505604098506,1.3685546875,2.1));
#18280=CARTESIAN_POINT('Origin',(5.5,1.6,2.1));
#18281=CARTESIAN_POINT('',(5.79505604098506,1.3685546875,1.5));
#18282=CARTESIAN_POINT('',(5.79505604098506,1.3685546875,1.5));
#18283=CARTESIAN_POINT('Origin',(5.5,1.6,1.5));
#18284=CARTESIAN_POINT('Origin',(5.5,1.6,2.1));
#18285=CARTESIAN_POINT('Origin',(5.5,0.,2.1));
#18286=CARTESIAN_POINT('Origin',(5.5,0.,1.5));
#18287=CARTESIAN_POINT('',(3.5,-2.44929359829471E-16,1.5));
#18288=CARTESIAN_POINT('Origin',(5.5,0.,1.5));
#18289=CARTESIAN_POINT('',(4.1,-1.71450551880629E-16,1.5));
#18290=CARTESIAN_POINT('Origin',(5.5,0.,1.5));
#18291=CARTESIAN_POINT('Origin',(5.5,0.,1.5));
#18292=CARTESIAN_POINT('Origin',(5.5,0.,1.5));
#18293=CARTESIAN_POINT('',(5.275,-1.6,1.5));
#18294=CARTESIAN_POINT('Origin',(5.5,-1.6,1.5));
#18295=CARTESIAN_POINT('',(5.275,1.6,1.5));
#18296=CARTESIAN_POINT('Origin',(5.5,1.6,1.5));
#18297=CARTESIAN_POINT('Origin',(6.09,0.,2.));
#18298=CARTESIAN_POINT('',(6.09,0.133884278389961,1.90356349239007));
#18299=CARTESIAN_POINT('',(6.09,0.133884278389961,2.09643650760993));
#18300=CARTESIAN_POINT('',(6.09,0.133884278389961,1.));
#18301=CARTESIAN_POINT('Origin',(6.09,0.,2.));
#18302=CARTESIAN_POINT('Origin',(6.09,0.,2.));
#18303=CARTESIAN_POINT('',(6.09,-0.133884278389961,1.90356349239007));
#18304=CARTESIAN_POINT('Ctrl Pts',(6.09,-0.133884278389961,1.90356349239007));
#18305=CARTESIAN_POINT('Ctrl Pts',(6.09119840340611,-0.128603165341395,
1.89623164237677));
#18306=CARTESIAN_POINT('Ctrl Pts',(6.09244064128815,-0.122792448979944,
1.88944721118838));
#18307=CARTESIAN_POINT('Ctrl Pts',(6.09651064111414,-0.10208383195986,1.8687385941683));
#18308=CARTESIAN_POINT('Ctrl Pts',(6.09954409498317,-0.0836002135946606,
1.8560565239921));
#18309=CARTESIAN_POINT('Ctrl Pts',(6.10381707438298,-0.0429774150042654,
1.8391843843662));
#18310=CARTESIAN_POINT('Ctrl Pts',(6.105,-0.0208299403327843,1.835));
#18311=CARTESIAN_POINT('Ctrl Pts',(6.105,0.0208299403327842,1.835));
#18312=CARTESIAN_POINT('Ctrl Pts',(6.10381707438298,0.0429774150042654,
1.8391843843662));
#18313=CARTESIAN_POINT('Ctrl Pts',(6.09954409498317,0.0836002135946606,
1.8560565239921));
#18314=CARTESIAN_POINT('Ctrl Pts',(6.09651064111414,0.10208383195986,1.8687385941683));
#18315=CARTESIAN_POINT('Ctrl Pts',(6.09244064128815,0.122792448979944,1.88944721118838));
#18316=CARTESIAN_POINT('Ctrl Pts',(6.09119840340611,0.128603165341395,1.89623164237677));
#18317=CARTESIAN_POINT('Ctrl Pts',(6.09,0.133884278389961,1.90356349239007));
#18318=CARTESIAN_POINT('',(6.09,-0.133884278389961,2.09643650760993));
#18319=CARTESIAN_POINT('Origin',(6.09,0.,2.));
#18320=CARTESIAN_POINT('',(6.105,-3.4389464756641E-17,2.165));
#18321=CARTESIAN_POINT('Ctrl Pts',(6.105,-4.85722573273506E-17,2.165));
#18322=CARTESIAN_POINT('Ctrl Pts',(6.105,-0.0208299403327842,2.165));
#18323=CARTESIAN_POINT('Ctrl Pts',(6.10381707438298,-0.0429774150042653,
2.1608156156338));
#18324=CARTESIAN_POINT('Ctrl Pts',(6.09954409498317,-0.0836002135946605,
2.1439434760079));
#18325=CARTESIAN_POINT('Ctrl Pts',(6.09651064111414,-0.10208383195986,2.1312614058317));
#18326=CARTESIAN_POINT('Ctrl Pts',(6.09244064128815,-0.122792448979944,
2.11055278881162));
#18327=CARTESIAN_POINT('Ctrl Pts',(6.09119840340611,-0.128603165341395,
2.10376835762323));
#18328=CARTESIAN_POINT('Ctrl Pts',(6.09,-0.133884278389961,2.09643650760993));
#18329=CARTESIAN_POINT('',(6.9,-2.02066721859313E-17,2.165));
#18330=CARTESIAN_POINT('',(6.09,-2.02066721859313E-17,2.165));
#18331=CARTESIAN_POINT('',(6.8902427845524,0.165,2.));
#18332=CARTESIAN_POINT('Ctrl Pts',(6.8902427845524,0.165,2.));
#18333=CARTESIAN_POINT('Ctrl Pts',(6.8902427845524,0.165,1.97926146026001));
#18334=CARTESIAN_POINT('Ctrl Pts',(6.89075468722975,0.16085144747456,1.95715388604164));
#18335=CARTESIAN_POINT('Ctrl Pts',(6.89259968365095,0.144006627864301,1.9165070705051));
#18336=CARTESIAN_POINT('Ctrl Pts',(6.89390570229761,0.131311408395222,1.89796617060366));
#18337=CARTESIAN_POINT('Ctrl Pts',(6.89635413416378,0.102033925885227,1.86868868809367));
#18338=CARTESIAN_POINT('Ctrl Pts',(6.89765618378145,0.0834929839417279,
1.85599339308932));
#18339=CARTESIAN_POINT('Ctrl Pts',(6.89949208802221,0.0428460264460561,
1.83914851786885));
#18340=CARTESIAN_POINT('Ctrl Pts',(6.9,0.0207384030457214,1.835));
#18341=CARTESIAN_POINT('Ctrl Pts',(6.9,-0.0207384030457214,1.835));
#18342=CARTESIAN_POINT('Ctrl Pts',(6.89949208802221,-0.042846026446056,
1.83914851786885));
#18343=CARTESIAN_POINT('Ctrl Pts',(6.89765618378145,-0.0834929839417279,
1.85599339308932));
#18344=CARTESIAN_POINT('Ctrl Pts',(6.89635413416378,-0.102033925885227,
1.86868868809367));
#18345=CARTESIAN_POINT('Ctrl Pts',(6.89390570229761,-0.131311408395222,
1.89796617060366));
#18346=CARTESIAN_POINT('Ctrl Pts',(6.89259968365095,-0.144006627864301,
1.9165070705051));
#18347=CARTESIAN_POINT('Ctrl Pts',(6.89075468722975,-0.16085144747456,1.95715388604164));
#18348=CARTESIAN_POINT('Ctrl Pts',(6.8902427845524,-0.165,1.97926146026001));
#18349=CARTESIAN_POINT('Ctrl Pts',(6.8902427845524,-0.165,2.02073853973999));
#18350=CARTESIAN_POINT('Ctrl Pts',(6.89075468722975,-0.160851447474559,
2.04284611395836));
#18351=CARTESIAN_POINT('Ctrl Pts',(6.89259968365095,-0.144006627864301,
2.0834929294949));
#18352=CARTESIAN_POINT('Ctrl Pts',(6.89390570229761,-0.131311408395222,
2.10203382939634));
#18353=CARTESIAN_POINT('Ctrl Pts',(6.89635413416378,-0.102033925885227,
2.13131131190633));
#18354=CARTESIAN_POINT('Ctrl Pts',(6.89765618378145,-0.0834929839417278,
2.14400660691068));
#18355=CARTESIAN_POINT('Ctrl Pts',(6.89949208802221,-0.0428460264460559,
2.16085148213115));
#18356=CARTESIAN_POINT('Ctrl Pts',(6.9,-0.0207384030457214,2.165));
#18357=CARTESIAN_POINT('Ctrl Pts',(6.9,-6.24500451351651E-17,2.165));
#18358=CARTESIAN_POINT('Ctrl Pts',(6.9,-2.42861286636753E-17,2.165));
#18359=CARTESIAN_POINT('Ctrl Pts',(6.9,0.0207384030457214,2.165));
#18360=CARTESIAN_POINT('Ctrl Pts',(6.89949208802221,0.0428460264460559,
2.16085148213115));
#18361=CARTESIAN_POINT('Ctrl Pts',(6.89765618378145,0.0834929839417279,
2.14400660691068));
#18362=CARTESIAN_POINT('Ctrl Pts',(6.89635413416378,0.102033925885227,2.13131131190633));
#18363=CARTESIAN_POINT('Ctrl Pts',(6.89390570229761,0.131311408395222,2.10203382939634));
#18364=CARTESIAN_POINT('Ctrl Pts',(6.89259968365095,0.144006627864301,2.0834929294949));
#18365=CARTESIAN_POINT('Ctrl Pts',(6.89075468722975,0.160851447474559,2.04284611395836));
#18366=CARTESIAN_POINT('Ctrl Pts',(6.8902427845524,0.165,2.02073853973999));
#18367=CARTESIAN_POINT('Ctrl Pts',(6.8902427845524,0.165,2.));
#18368=CARTESIAN_POINT('Ctrl Pts',(6.09,0.133884278389961,2.09643650760993));
#18369=CARTESIAN_POINT('Ctrl Pts',(6.09119840340611,0.128603165341395,2.10376835762323));
#18370=CARTESIAN_POINT('Ctrl Pts',(6.09244064128815,0.122792448979944,2.11055278881162));
#18371=CARTESIAN_POINT('Ctrl Pts',(6.09651064111414,0.10208383195986,2.1312614058317));
#18372=CARTESIAN_POINT('Ctrl Pts',(6.09954409498317,0.0836002135946605,
2.1439434760079));
#18373=CARTESIAN_POINT('Ctrl Pts',(6.10381707438298,0.0429774150042653,
2.1608156156338));
#18374=CARTESIAN_POINT('Ctrl Pts',(6.105,0.0208299403327843,2.165));
#18375=CARTESIAN_POINT('Ctrl Pts',(6.105,6.24500451351651E-17,2.165));
#18376=CARTESIAN_POINT('Origin',(6.09,0.,2.));
#18377=CARTESIAN_POINT('',(6.09,-0.133884278389961,1.));
#18378=CARTESIAN_POINT('Origin',(5.5,-1.6,0.9));
#18379=CARTESIAN_POINT('',(5.275,-1.6,1.));
#18380=CARTESIAN_POINT('Origin',(5.5,-1.6,1.));
#18381=CARTESIAN_POINT('',(5.275,-1.6,0.9));
#18382=CARTESIAN_POINT('Origin',(5.5,1.6,0.9));
#18383=CARTESIAN_POINT('',(5.275,1.6,1.));
#18384=CARTESIAN_POINT('Origin',(5.5,1.6,1.));
#18385=CARTESIAN_POINT('',(5.275,1.6,0.9));
#18386=CARTESIAN_POINT('Origin',(5.5,0.,1.5));
#18387=CARTESIAN_POINT('',(4.1,-1.71450551880629E-16,2.5));
#18388=CARTESIAN_POINT('Origin',(5.5,0.,2.5));
#18389=CARTESIAN_POINT('',(4.1,-1.71450551880629E-16,1.5));
#18390=CARTESIAN_POINT('Origin',(5.5,0.,2.5));
#18391=CARTESIAN_POINT('',(4.895,-7.40911313484149E-17,2.5));
#18392=CARTESIAN_POINT('Origin',(5.5,0.,2.5));
#18393=CARTESIAN_POINT('Origin',(5.5,0.,1.));
#18394=CARTESIAN_POINT('',(4.895,-7.40911313484149E-17,1.));
#18395=CARTESIAN_POINT('',(4.895,-7.40911313484149E-17,1.));
#18396=CARTESIAN_POINT('Origin',(5.5,0.,1.));
#18397=CARTESIAN_POINT('Origin',(5.5,0.,1.));
#18398=CARTESIAN_POINT('',(3.5,-2.44929359829471E-16,1.));
#18399=CARTESIAN_POINT('',(3.5,-2.44929359829471E-16,1.));
#18400=CARTESIAN_POINT('Origin',(5.5,0.,1.));
#18401=CARTESIAN_POINT('Origin',(5.5,0.,1.));
#18402=CARTESIAN_POINT('',(0.,0.,0.));
#18403=CARTESIAN_POINT('Origin',(0.21,-1.01,12.9));
#18404=CARTESIAN_POINT('',(0.21,-1.01,13.));
#18405=CARTESIAN_POINT('',(0.21,-0.621228621362538,13.));
#18406=CARTESIAN_POINT('',(0.21,-0.505,13.));
#18407=CARTESIAN_POINT('',(0.21,-1.01,15.3));
#18408=CARTESIAN_POINT('',(0.21,-1.01,12.9));
#18409=CARTESIAN_POINT('',(0.21,-0.621228621362538,15.3));
#18410=CARTESIAN_POINT('',(0.21,-0.505,15.3));
#18411=CARTESIAN_POINT('',(0.21,-0.621228621362538,13.));
#18412=CARTESIAN_POINT('Origin',(0.21,-1.01,12.9));
#18413=CARTESIAN_POINT('',(0.21,1.01,15.3));
#18414=CARTESIAN_POINT('',(0.21,0.621228621362538,15.3));
#18415=CARTESIAN_POINT('',(0.21,-0.505,15.3));
#18416=CARTESIAN_POINT('',(0.21,1.01,13.));
#18417=CARTESIAN_POINT('',(0.21,1.01,12.9));
#18418=CARTESIAN_POINT('',(0.21,0.621228621362538,13.));
#18419=CARTESIAN_POINT('',(0.21,-0.505,13.));
#18420=CARTESIAN_POINT('',(0.21,0.621228621362538,13.));
#18421=CARTESIAN_POINT('Origin',(0.21,1.01,12.9));
#18422=CARTESIAN_POINT('',(-0.240927072796786,1.01,15.3));
#18423=CARTESIAN_POINT('',(0.605,1.01,15.3));
#18424=CARTESIAN_POINT('',(-0.240927072796786,1.01,15.));
#18425=CARTESIAN_POINT('',(-0.240927072796786,1.01,15.));
#18426=CARTESIAN_POINT('',(0.0305156009506911,1.01,15.));
#18427=CARTESIAN_POINT('',(0.605,1.01,15.));
#18428=CARTESIAN_POINT('',(0.0305156009506911,1.01,13.));
#18429=CARTESIAN_POINT('',(0.0305156009506911,1.01,13.));
#18430=CARTESIAN_POINT('',(0.605,1.01,13.));
#18431=CARTESIAN_POINT('Origin',(-0.7,-1.01,12.9));
#18432=CARTESIAN_POINT('',(0.0305156009506911,-1.01,13.));
#18433=CARTESIAN_POINT('',(0.15,-1.01,13.));
#18434=CARTESIAN_POINT('',(0.0305156009506911,-1.01,15.));
#18435=CARTESIAN_POINT('',(0.0305156009506911,-1.01,13.));
#18436=CARTESIAN_POINT('',(-0.240927072796786,-1.01,15.));
#18437=CARTESIAN_POINT('',(0.15,-1.01,15.));
#18438=CARTESIAN_POINT('',(-0.240927072796786,-1.01,15.3));
#18439=CARTESIAN_POINT('',(-0.240927072796786,-1.01,15.));
#18440=CARTESIAN_POINT('',(0.15,-1.01,15.3));
#18441=CARTESIAN_POINT('Origin',(1.,0.,13.));
#18442=CARTESIAN_POINT('Origin',(1.,0.,13.));
#18443=CARTESIAN_POINT('Origin',(1.,0.,13.));
#18444=CARTESIAN_POINT('Origin',(1.,0.,13.));
#18445=CARTESIAN_POINT('Origin',(1.,0.,15.3));
#18446=CARTESIAN_POINT('Origin',(1.,0.,13.));
#18447=CARTESIAN_POINT('Origin',(1.,0.,15.));
#18448=CARTESIAN_POINT('Origin',(1.,0.,15.));
#18449=CARTESIAN_POINT('Origin',(1.,0.,15.));
#18450=CARTESIAN_POINT('Origin',(1.,0.,15.));
#18451=CARTESIAN_POINT('Origin',(1.,0.,15.3));
#18452=CARTESIAN_POINT('Origin',(1.,0.,15.3));
#18453=CARTESIAN_POINT('',(0.,0.,0.));
#18454=CARTESIAN_POINT('Origin',(2.4,-1.6,15.2));
#18455=CARTESIAN_POINT('',(2.175,-1.6,15.3));
#18456=CARTESIAN_POINT('Origin',(2.4,-1.6,15.3));
#18457=CARTESIAN_POINT('',(2.175,-1.6,15.6));
#18458=CARTESIAN_POINT('',(2.175,-1.6,15.2));
#18459=CARTESIAN_POINT('Origin',(2.4,-1.6,15.6));
#18460=CARTESIAN_POINT('Origin',(2.4,1.6,15.2));
#18461=CARTESIAN_POINT('',(2.175,1.6,15.3));
#18462=CARTESIAN_POINT('Origin',(2.4,1.6,15.3));
#18463=CARTESIAN_POINT('',(2.175,1.6,15.6));
#18464=CARTESIAN_POINT('',(2.175,1.6,15.2));
#18465=CARTESIAN_POINT('Origin',(2.4,1.6,15.6));
#18466=CARTESIAN_POINT('Origin',(0.21,1.01,15.2));
#18467=CARTESIAN_POINT('',(0.21,1.01,15.3));
#18468=CARTESIAN_POINT('',(0.,1.01,15.3));
#18469=CARTESIAN_POINT('',(0.905,1.01,15.3));
#18470=CARTESIAN_POINT('',(0.21,1.01,15.6));
#18471=CARTESIAN_POINT('',(0.21,1.01,15.2));
#18472=CARTESIAN_POINT('',(0.,1.01,15.6));
#18473=CARTESIAN_POINT('',(0.905,1.01,15.6));
#18474=CARTESIAN_POINT('',(0.,1.01,15.25));
#18475=CARTESIAN_POINT('Origin',(-0.1,-1.01,15.2));
#18476=CARTESIAN_POINT('',(0.21,-1.01,15.6));
#18477=CARTESIAN_POINT('',(0.,-1.01,15.6));
#18478=CARTESIAN_POINT('',(0.75,-1.01,15.6));
#18479=CARTESIAN_POINT('',(0.21,-1.01,15.3));
#18480=CARTESIAN_POINT('',(0.21,-1.01,15.2));
#18481=CARTESIAN_POINT('',(0.,-1.01,15.3));
#18482=CARTESIAN_POINT('',(0.75,-1.01,15.3));
#18483=CARTESIAN_POINT('',(0.,-1.01,15.25));
#18484=CARTESIAN_POINT('Origin',(0.21,-1.01,15.2));
#18485=CARTESIAN_POINT('',(0.21,-0.629285308902091,15.6));
#18486=CARTESIAN_POINT('',(0.21,-0.505,15.6));
#18487=CARTESIAN_POINT('',(0.21,-0.629285308902091,15.3));
#18488=CARTESIAN_POINT('',(0.21,-0.629285308902091,15.2));
#18489=CARTESIAN_POINT('',(0.21,-0.505,15.3));
#18490=CARTESIAN_POINT('Origin',(0.21,-1.01,15.2));
#18491=CARTESIAN_POINT('',(0.21,0.629285308902091,15.3));
#18492=CARTESIAN_POINT('',(0.21,-0.505,15.3));
#18493=CARTESIAN_POINT('',(0.21,0.629285308902091,15.6));
#18494=CARTESIAN_POINT('',(0.21,0.629285308902091,15.2));
#18495=CARTESIAN_POINT('',(0.21,-0.505,15.6));
#18496=CARTESIAN_POINT('Origin',(0.,2.2,15.3));
#18497=CARTESIAN_POINT('',(0.,2.2,15.6));
#18498=CARTESIAN_POINT('',(0.,2.2,15.6));
#18499=CARTESIAN_POINT('',(0.,2.2,15.3));
#18500=CARTESIAN_POINT('',(0.,2.2,15.3));
#18501=CARTESIAN_POINT('',(0.,2.2,15.3));
#18502=CARTESIAN_POINT('Origin',(0.,2.2,15.3));
#18503=CARTESIAN_POINT('',(0.,-2.2,15.3));
#18504=CARTESIAN_POINT('',(0.,2.2,15.3));
#18505=CARTESIAN_POINT('',(0.,-2.2,15.6));
#18506=CARTESIAN_POINT('',(0.,-2.2,15.3));
#18507=CARTESIAN_POINT('',(0.,2.2,15.6));
#18508=CARTESIAN_POINT('Origin',(1.6,0.,15.6));
#18509=CARTESIAN_POINT('Origin',(1.,0.,15.6));
#18510=CARTESIAN_POINT('',(3.2,-2.2,15.6));
#18511=CARTESIAN_POINT('',(0.,-2.2,15.6));
#18512=CARTESIAN_POINT('',(3.2,2.2,15.6));
#18513=CARTESIAN_POINT('',(3.2,-2.2,15.6));
#18514=CARTESIAN_POINT('',(3.2,2.2,15.6));
#18515=CARTESIAN_POINT('Origin',(1.,0.,15.2));
#18516=CARTESIAN_POINT('Origin',(1.,0.,15.3));
#18517=CARTESIAN_POINT('Origin',(3.2,2.2,15.3));
#18518=CARTESIAN_POINT('',(3.2,2.2,15.3));
#18519=CARTESIAN_POINT('',(3.2,2.2,15.3));
#18520=CARTESIAN_POINT('',(3.2,2.2,15.3));
#18521=CARTESIAN_POINT('Origin',(3.2,-2.2,15.3));
#18522=CARTESIAN_POINT('',(3.2,-2.2,15.3));
#18523=CARTESIAN_POINT('',(3.2,-2.2,15.3));
#18524=CARTESIAN_POINT('',(3.2,-2.2,15.3));
#18525=CARTESIAN_POINT('Origin',(0.,-2.2,15.3));
#18526=CARTESIAN_POINT('',(0.,-2.2,15.3));
#18527=CARTESIAN_POINT('Origin',(1.6,0.,15.3));
#18528=CARTESIAN_POINT('',(0.,0.,0.));
#18529=CARTESIAN_POINT('Origin',(0.21,-1.01,22.9));
#18530=CARTESIAN_POINT('',(0.21,-1.01,23.));
#18531=CARTESIAN_POINT('',(0.21,-0.621228621362538,23.));
#18532=CARTESIAN_POINT('',(0.21,-0.505,23.));
#18533=CARTESIAN_POINT('',(0.21,-1.01,25.3));
#18534=CARTESIAN_POINT('',(0.21,-1.01,22.9));
#18535=CARTESIAN_POINT('',(0.21,-0.621228621362538,25.3));
#18536=CARTESIAN_POINT('',(0.21,-0.505,25.3));
#18537=CARTESIAN_POINT('',(0.21,-0.621228621362538,23.));
#18538=CARTESIAN_POINT('Origin',(0.21,-1.01,22.9));
#18539=CARTESIAN_POINT('',(0.21,1.01,25.3));
#18540=CARTESIAN_POINT('',(0.21,0.621228621362538,25.3));
#18541=CARTESIAN_POINT('',(0.21,-0.505,25.3));
#18542=CARTESIAN_POINT('',(0.21,1.01,23.));
#18543=CARTESIAN_POINT('',(0.21,1.01,22.9));
#18544=CARTESIAN_POINT('',(0.21,0.621228621362538,23.));
#18545=CARTESIAN_POINT('',(0.21,-0.505,23.));
#18546=CARTESIAN_POINT('',(0.21,0.621228621362538,23.));
#18547=CARTESIAN_POINT('Origin',(0.21,1.01,22.9));
#18548=CARTESIAN_POINT('',(-0.240927072796786,1.01,25.3));
#18549=CARTESIAN_POINT('',(0.605,1.01,25.3));
#18550=CARTESIAN_POINT('',(-0.240927072796786,1.01,25.));
#18551=CARTESIAN_POINT('',(-0.240927072796786,1.01,25.));
#18552=CARTESIAN_POINT('',(0.0305156009506911,1.01,25.));
#18553=CARTESIAN_POINT('',(0.605,1.01,25.));
#18554=CARTESIAN_POINT('',(0.0305156009506911,1.01,23.));
#18555=CARTESIAN_POINT('',(0.0305156009506911,1.01,23.));
#18556=CARTESIAN_POINT('',(0.605,1.01,23.));
#18557=CARTESIAN_POINT('Origin',(-0.7,-1.01,22.9));
#18558=CARTESIAN_POINT('',(0.0305156009506911,-1.01,23.));
#18559=CARTESIAN_POINT('',(0.15,-1.01,23.));
#18560=CARTESIAN_POINT('',(0.0305156009506911,-1.01,25.));
#18561=CARTESIAN_POINT('',(0.0305156009506911,-1.01,23.));
#18562=CARTESIAN_POINT('',(-0.240927072796786,-1.01,25.));
#18563=CARTESIAN_POINT('',(0.15,-1.01,25.));
#18564=CARTESIAN_POINT('',(-0.240927072796786,-1.01,25.3));
#18565=CARTESIAN_POINT('',(-0.240927072796786,-1.01,25.));
#18566=CARTESIAN_POINT('',(0.15,-1.01,25.3));
#18567=CARTESIAN_POINT('Origin',(1.,0.,23.));
#18568=CARTESIAN_POINT('Origin',(1.,0.,23.));
#18569=CARTESIAN_POINT('Origin',(1.,0.,23.));
#18570=CARTESIAN_POINT('Origin',(1.,0.,23.));
#18571=CARTESIAN_POINT('Origin',(1.,0.,25.3));
#18572=CARTESIAN_POINT('Origin',(1.,0.,23.));
#18573=CARTESIAN_POINT('Origin',(1.,0.,25.));
#18574=CARTESIAN_POINT('Origin',(1.,0.,25.));
#18575=CARTESIAN_POINT('Origin',(1.,0.,25.));
#18576=CARTESIAN_POINT('Origin',(1.,0.,25.));
#18577=CARTESIAN_POINT('Origin',(1.,0.,25.3));
#18578=CARTESIAN_POINT('Origin',(1.,0.,25.3));
#18579=CARTESIAN_POINT('',(0.,0.,0.));
#18580=CARTESIAN_POINT('Origin',(2.4,-1.6,25.2));
#18581=CARTESIAN_POINT('',(2.175,-1.6,25.3));
#18582=CARTESIAN_POINT('Origin',(2.4,-1.6,25.3));
#18583=CARTESIAN_POINT('',(2.175,-1.6,25.6));
#18584=CARTESIAN_POINT('',(2.175,-1.6,25.2));
#18585=CARTESIAN_POINT('Origin',(2.4,-1.6,25.6));
#18586=CARTESIAN_POINT('Origin',(2.4,1.6,25.2));
#18587=CARTESIAN_POINT('',(2.175,1.6,25.3));
#18588=CARTESIAN_POINT('Origin',(2.4,1.6,25.3));
#18589=CARTESIAN_POINT('',(2.175,1.6,25.6));
#18590=CARTESIAN_POINT('',(2.175,1.6,25.2));
#18591=CARTESIAN_POINT('Origin',(2.4,1.6,25.6));
#18592=CARTESIAN_POINT('Origin',(0.21,1.01,25.2));
#18593=CARTESIAN_POINT('',(0.21,1.01,25.3));
#18594=CARTESIAN_POINT('',(0.,1.01,25.3));
#18595=CARTESIAN_POINT('',(0.905,1.01,25.3));
#18596=CARTESIAN_POINT('',(0.21,1.01,25.6));
#18597=CARTESIAN_POINT('',(0.21,1.01,25.2));
#18598=CARTESIAN_POINT('',(0.,1.01,25.6));
#18599=CARTESIAN_POINT('',(0.905,1.01,25.6));
#18600=CARTESIAN_POINT('',(0.,1.01,25.25));
#18601=CARTESIAN_POINT('Origin',(-0.1,-1.01,25.2));
#18602=CARTESIAN_POINT('',(0.21,-1.01,25.6));
#18603=CARTESIAN_POINT('',(0.,-1.01,25.6));
#18604=CARTESIAN_POINT('',(0.75,-1.01,25.6));
#18605=CARTESIAN_POINT('',(0.21,-1.01,25.3));
#18606=CARTESIAN_POINT('',(0.21,-1.01,25.2));
#18607=CARTESIAN_POINT('',(0.,-1.01,25.3));
#18608=CARTESIAN_POINT('',(0.75,-1.01,25.3));
#18609=CARTESIAN_POINT('',(0.,-1.01,25.25));
#18610=CARTESIAN_POINT('Origin',(0.21,-1.01,25.2));
#18611=CARTESIAN_POINT('',(0.21,-0.629285308902091,25.6));
#18612=CARTESIAN_POINT('',(0.21,-0.505,25.6));
#18613=CARTESIAN_POINT('',(0.21,-0.629285308902091,25.3));
#18614=CARTESIAN_POINT('',(0.21,-0.629285308902091,25.2));
#18615=CARTESIAN_POINT('',(0.21,-0.505,25.3));
#18616=CARTESIAN_POINT('Origin',(0.21,-1.01,25.2));
#18617=CARTESIAN_POINT('',(0.21,0.629285308902091,25.3));
#18618=CARTESIAN_POINT('',(0.21,-0.505,25.3));
#18619=CARTESIAN_POINT('',(0.21,0.629285308902091,25.6));
#18620=CARTESIAN_POINT('',(0.21,0.629285308902091,25.2));
#18621=CARTESIAN_POINT('',(0.21,-0.505,25.6));
#18622=CARTESIAN_POINT('Origin',(0.,2.2,25.3));
#18623=CARTESIAN_POINT('',(0.,2.2,25.6));
#18624=CARTESIAN_POINT('',(0.,2.2,25.6));
#18625=CARTESIAN_POINT('',(0.,2.2,25.3));
#18626=CARTESIAN_POINT('',(0.,2.2,25.3));
#18627=CARTESIAN_POINT('',(0.,2.2,25.3));
#18628=CARTESIAN_POINT('Origin',(0.,2.2,25.3));
#18629=CARTESIAN_POINT('',(0.,-2.2,25.3));
#18630=CARTESIAN_POINT('',(0.,2.2,25.3));
#18631=CARTESIAN_POINT('',(0.,-2.2,25.6));
#18632=CARTESIAN_POINT('',(0.,-2.2,25.3));
#18633=CARTESIAN_POINT('',(0.,2.2,25.6));
#18634=CARTESIAN_POINT('Origin',(1.6,0.,25.6));
#18635=CARTESIAN_POINT('Origin',(1.,0.,25.6));
#18636=CARTESIAN_POINT('',(3.2,-2.2,25.6));
#18637=CARTESIAN_POINT('',(0.,-2.2,25.6));
#18638=CARTESIAN_POINT('',(3.2,2.2,25.6));
#18639=CARTESIAN_POINT('',(3.2,-2.2,25.6));
#18640=CARTESIAN_POINT('',(3.2,2.2,25.6));
#18641=CARTESIAN_POINT('Origin',(1.,0.,25.2));
#18642=CARTESIAN_POINT('Origin',(1.,0.,25.3));
#18643=CARTESIAN_POINT('Origin',(3.2,2.2,25.3));
#18644=CARTESIAN_POINT('',(3.2,2.2,25.3));
#18645=CARTESIAN_POINT('',(3.2,2.2,25.3));
#18646=CARTESIAN_POINT('',(3.2,2.2,25.3));
#18647=CARTESIAN_POINT('Origin',(3.2,-2.2,25.3));
#18648=CARTESIAN_POINT('',(3.2,-2.2,25.3));
#18649=CARTESIAN_POINT('',(3.2,-2.2,25.3));
#18650=CARTESIAN_POINT('',(3.2,-2.2,25.3));
#18651=CARTESIAN_POINT('Origin',(0.,-2.2,25.3));
#18652=CARTESIAN_POINT('',(0.,-2.2,25.3));
#18653=CARTESIAN_POINT('Origin',(1.6,0.,25.3));
#18654=CARTESIAN_POINT('',(0.,0.,0.));
#18655=CARTESIAN_POINT('Origin',(-0.5,2.,4.4));
#18656=CARTESIAN_POINT('',(7.,2.,5.5));
#18657=CARTESIAN_POINT('',(-0.5,2.,5.5));
#18658=CARTESIAN_POINT('',(0.5,2.,5.5));
#18659=CARTESIAN_POINT('',(7.,2.,4.5));
#18660=CARTESIAN_POINT('',(7.,2.,4.45));
#18661=CARTESIAN_POINT('',(-0.5,2.,4.5));
#18662=CARTESIAN_POINT('',(0.5,2.,4.5));
#18663=CARTESIAN_POINT('',(-0.5,2.,4.4));
#18664=CARTESIAN_POINT('Origin',(-0.5,-4.1,4.4));
#18665=CARTESIAN_POINT('',(-0.5,-2.,4.5));
#18666=CARTESIAN_POINT('',(-0.5,-2.05,4.5));
#18667=CARTESIAN_POINT('',(-0.5,-2.,5.5));
#18668=CARTESIAN_POINT('',(-0.5,-2.,4.4));
#18669=CARTESIAN_POINT('',(-0.5,-2.05,5.5));
#18670=CARTESIAN_POINT('Origin',(1.5,0.,4.5));
#18671=CARTESIAN_POINT('',(7.,-2.,4.5));
#18672=CARTESIAN_POINT('',(7.,-4.,4.5));
#18673=CARTESIAN_POINT('',(4.3,-2.,4.5));
#18674=CARTESIAN_POINT('',(0.5,-6.12323399573677E-17,4.5));
#18675=CARTESIAN_POINT('Origin',(1.,0.,4.5));
#18676=CARTESIAN_POINT('',(4.1,-1.71450551880629E-16,4.5));
#18677=CARTESIAN_POINT('Origin',(5.5,0.,4.5));
#18678=CARTESIAN_POINT('Origin',(7.1,-2.,4.4));
#18679=CARTESIAN_POINT('',(7.,-2.,5.5));
#18680=CARTESIAN_POINT('',(4.3,-2.,5.5));
#18681=CARTESIAN_POINT('',(7.,-2.,4.45));
#18682=CARTESIAN_POINT('Origin',(7.,-4.,4.5));
#18683=CARTESIAN_POINT('',(7.,-4.,5.5));
#18684=CARTESIAN_POINT('Origin',(1.5,0.,5.5));
#18685=CARTESIAN_POINT('',(4.895,7.40911313484149E-17,5.5));
#18686=CARTESIAN_POINT('Origin',(5.5,0.,5.5));
#18687=CARTESIAN_POINT('',(0.5,6.12323399573677E-17,5.5));
#18688=CARTESIAN_POINT('Origin',(1.,0.,5.5));
#18689=CARTESIAN_POINT('Origin',(6.09,0.,3.75));
#18690=CARTESIAN_POINT('',(6.09,0.133884278389961,3.65356349239007));
#18691=CARTESIAN_POINT('',(6.09,0.133884278389961,3.84643650760993));
#18692=CARTESIAN_POINT('',(6.09,0.133884278389961,2.9));
#18693=CARTESIAN_POINT('Origin',(6.09,0.,3.75));
#18694=CARTESIAN_POINT('Origin',(6.09,0.,3.75));
#18695=CARTESIAN_POINT('',(6.09,-0.133884278389961,3.65356349239007));
#18696=CARTESIAN_POINT('Ctrl Pts',(6.09,-0.133884278389961,3.65356349239007));
#18697=CARTESIAN_POINT('Ctrl Pts',(6.09119840340611,-0.128603165341395,
3.64623164237677));
#18698=CARTESIAN_POINT('Ctrl Pts',(6.09244064128815,-0.122792448979944,
3.63944721118838));
#18699=CARTESIAN_POINT('Ctrl Pts',(6.09651064111414,-0.10208383195986,3.6187385941683));
#18700=CARTESIAN_POINT('Ctrl Pts',(6.09954409498317,-0.0836002135946606,
3.6060565239921));
#18701=CARTESIAN_POINT('Ctrl Pts',(6.10381707438298,-0.0429774150042654,
3.5891843843662));
#18702=CARTESIAN_POINT('Ctrl Pts',(6.105,-0.0208299403327843,3.585));
#18703=CARTESIAN_POINT('Ctrl Pts',(6.105,0.0208299403327842,3.585));
#18704=CARTESIAN_POINT('Ctrl Pts',(6.10381707438298,0.0429774150042653,
3.5891843843662));
#18705=CARTESIAN_POINT('Ctrl Pts',(6.09954409498317,0.0836002135946605,
3.6060565239921));
#18706=CARTESIAN_POINT('Ctrl Pts',(6.09651064111414,0.10208383195986,3.6187385941683));
#18707=CARTESIAN_POINT('Ctrl Pts',(6.09244064128815,0.122792448979944,3.63944721118838));
#18708=CARTESIAN_POINT('Ctrl Pts',(6.09119840340611,0.128603165341395,3.64623164237677));
#18709=CARTESIAN_POINT('Ctrl Pts',(6.09,0.133884278389961,3.65356349239007));
#18710=CARTESIAN_POINT('',(6.09,-0.133884278389961,3.84643650760993));
#18711=CARTESIAN_POINT('Origin',(6.09,0.,3.75));
#18712=CARTESIAN_POINT('',(6.105,-4.82672525644554E-17,3.915));
#18713=CARTESIAN_POINT('Ctrl Pts',(6.105,-6.93889390390723E-17,3.915));
#18714=CARTESIAN_POINT('Ctrl Pts',(6.105,-0.0208299403327843,3.915));
#18715=CARTESIAN_POINT('Ctrl Pts',(6.10381707438298,-0.0429774150042653,
3.9108156156338));
#18716=CARTESIAN_POINT('Ctrl Pts',(6.09954409498317,-0.0836002135946605,
3.8939434760079));
#18717=CARTESIAN_POINT('Ctrl Pts',(6.09651064111414,-0.10208383195986,3.8812614058317));
#18718=CARTESIAN_POINT('Ctrl Pts',(6.09244064128815,-0.122792448979944,
3.86055278881162));
#18719=CARTESIAN_POINT('Ctrl Pts',(6.09119840340611,-0.128603165341395,
3.85376835762323));
#18720=CARTESIAN_POINT('Ctrl Pts',(6.09,-0.133884278389961,3.84643650760993));
#18721=CARTESIAN_POINT('',(6.9,-2.02066721859313E-17,3.915));
#18722=CARTESIAN_POINT('',(6.09,-2.02066721859313E-17,3.915));
#18723=CARTESIAN_POINT('',(6.8902427845524,0.165,3.75));
#18724=CARTESIAN_POINT('Ctrl Pts',(6.8902427845524,0.165,3.75));
#18725=CARTESIAN_POINT('Ctrl Pts',(6.8902427845524,0.165,3.72926146026001));
#18726=CARTESIAN_POINT('Ctrl Pts',(6.89075468722975,0.160851447474559,3.70715388604164));
#18727=CARTESIAN_POINT('Ctrl Pts',(6.89259968365095,0.144006627864301,3.6665070705051));
#18728=CARTESIAN_POINT('Ctrl Pts',(6.89390570229761,0.131311408395222,3.64796617060366));
#18729=CARTESIAN_POINT('Ctrl Pts',(6.89635413416378,0.102033925885227,3.61868868809367));
#18730=CARTESIAN_POINT('Ctrl Pts',(6.89765618378145,0.0834929839417279,
3.60599339308932));
#18731=CARTESIAN_POINT('Ctrl Pts',(6.89949208802221,0.0428460264460559,
3.58914851786885));
#18732=CARTESIAN_POINT('Ctrl Pts',(6.9,0.0207384030457214,3.585));
#18733=CARTESIAN_POINT('Ctrl Pts',(6.9,-0.0207384030457214,3.585));
#18734=CARTESIAN_POINT('Ctrl Pts',(6.89949208802221,-0.0428460264460559,
3.58914851786885));
#18735=CARTESIAN_POINT('Ctrl Pts',(6.89765618378145,-0.0834929839417279,
3.60599339308932));
#18736=CARTESIAN_POINT('Ctrl Pts',(6.89635413416378,-0.102033925885227,
3.61868868809367));
#18737=CARTESIAN_POINT('Ctrl Pts',(6.89390570229761,-0.131311408395222,
3.64796617060366));
#18738=CARTESIAN_POINT('Ctrl Pts',(6.89259968365095,-0.144006627864301,
3.6665070705051));
#18739=CARTESIAN_POINT('Ctrl Pts',(6.89075468722975,-0.160851447474559,
3.70715388604164));
#18740=CARTESIAN_POINT('Ctrl Pts',(6.8902427845524,-0.165,3.72926146026001));
#18741=CARTESIAN_POINT('Ctrl Pts',(6.8902427845524,-0.165,3.77073853973999));
#18742=CARTESIAN_POINT('Ctrl Pts',(6.89075468722975,-0.160851447474559,
3.79284611395836));
#18743=CARTESIAN_POINT('Ctrl Pts',(6.89259968365095,-0.144006627864301,
3.8334929294949));
#18744=CARTESIAN_POINT('Ctrl Pts',(6.89390570229761,-0.131311408395222,
3.85203382939634));
#18745=CARTESIAN_POINT('Ctrl Pts',(6.89635413416378,-0.102033925885227,
3.88131131190633));
#18746=CARTESIAN_POINT('Ctrl Pts',(6.89765618378145,-0.0834929839417278,
3.89400660691068));
#18747=CARTESIAN_POINT('Ctrl Pts',(6.89949208802221,-0.0428460264460559,
3.91085148213115));
#18748=CARTESIAN_POINT('Ctrl Pts',(6.9,-0.0207384030457214,3.915));
#18749=CARTESIAN_POINT('Ctrl Pts',(6.9,-7.63278329429795E-17,3.915));
#18750=CARTESIAN_POINT('Ctrl Pts',(6.9,-3.46944695195361E-17,3.915));
#18751=CARTESIAN_POINT('Ctrl Pts',(6.9,0.0207384030457214,3.915));
#18752=CARTESIAN_POINT('Ctrl Pts',(6.89949208802221,0.0428460264460559,
3.91085148213115));
#18753=CARTESIAN_POINT('Ctrl Pts',(6.89765618378145,0.0834929839417279,
3.89400660691068));
#18754=CARTESIAN_POINT('Ctrl Pts',(6.89635413416378,0.102033925885227,3.88131131190633));
#18755=CARTESIAN_POINT('Ctrl Pts',(6.89390570229761,0.131311408395222,3.85203382939634));
#18756=CARTESIAN_POINT('Ctrl Pts',(6.89259968365095,0.144006627864301,3.8334929294949));
#18757=CARTESIAN_POINT('Ctrl Pts',(6.89075468722975,0.160851447474559,3.79284611395836));
#18758=CARTESIAN_POINT('Ctrl Pts',(6.8902427845524,0.165,3.77073853973999));
#18759=CARTESIAN_POINT('Ctrl Pts',(6.8902427845524,0.165,3.75));
#18760=CARTESIAN_POINT('Ctrl Pts',(6.09,0.133884278389961,3.84643650760993));
#18761=CARTESIAN_POINT('Ctrl Pts',(6.09119840340611,0.128603165341395,3.85376835762323));
#18762=CARTESIAN_POINT('Ctrl Pts',(6.09244064128815,0.122792448979944,3.86055278881162));
#18763=CARTESIAN_POINT('Ctrl Pts',(6.09651064111414,0.10208383195986,3.8812614058317));
#18764=CARTESIAN_POINT('Ctrl Pts',(6.09954409498317,0.0836002135946605,
3.8939434760079));
#18765=CARTESIAN_POINT('Ctrl Pts',(6.10381707438298,0.0429774150042653,
3.9108156156338));
#18766=CARTESIAN_POINT('Ctrl Pts',(6.105,0.0208299403327843,3.915));
#18767=CARTESIAN_POINT('Ctrl Pts',(6.105,9.0205620750794E-17,3.915));
#18768=CARTESIAN_POINT('Origin',(6.09,0.,3.75));
#18769=CARTESIAN_POINT('',(6.09,-0.133884278389961,2.9));
#18770=CARTESIAN_POINT('Origin',(1.,0.,4.4));
#18771=CARTESIAN_POINT('',(0.5,-6.12323399573677E-17,4.4));
#18772=CARTESIAN_POINT('Origin',(5.5,0.,2.9));
#18773=CARTESIAN_POINT('',(4.895,-7.40911313484149E-17,3.));
#18774=CARTESIAN_POINT('Origin',(5.5,0.,3.));
#18775=CARTESIAN_POINT('',(4.895,-7.40911313484149E-17,2.9));
#18776=CARTESIAN_POINT('Origin',(5.5,0.,3.));
#18777=CARTESIAN_POINT('',(4.1,-1.71450551880629E-16,3.));
#18778=CARTESIAN_POINT('',(4.1,-1.71450551880629E-16,3.));
#18779=CARTESIAN_POINT('Origin',(5.5,0.,3.));
#18780=CARTESIAN_POINT('Origin',(5.5,0.,3.));
#18781=CARTESIAN_POINT('',(0.,0.,0.));
#18782=CARTESIAN_POINT('Origin',(-4.66421356237309,-3.9,18.5857864376269));
#18783=CARTESIAN_POINT('',(-4.82921356237309,-3.8,18.5857864376269));
#18784=CARTESIAN_POINT('Origin',(-4.66421356237309,-3.8,18.5857864376269));
#18785=CARTESIAN_POINT('',(-4.82921356237309,-2.2,18.5857864376269));
#18786=CARTESIAN_POINT('',(-4.82921356237309,-3.9,18.5857864376269));
#18787=CARTESIAN_POINT('Origin',(-4.66421356237309,-2.2,18.5857864376269));
#18788=CARTESIAN_POINT('Origin',(-4.66421356237309,-3.9,21.4142135623731));
#18789=CARTESIAN_POINT('',(-4.82921356237309,-3.8,21.4142135623731));
#18790=CARTESIAN_POINT('Origin',(-4.66421356237309,-3.8,21.4142135623731));
#18791=CARTESIAN_POINT('',(-4.82921356237309,-2.2,21.4142135623731));
#18792=CARTESIAN_POINT('',(-4.82921356237309,-3.9,21.4142135623731));
#18793=CARTESIAN_POINT('Origin',(-4.66421356237309,-2.2,21.4142135623731));
#18794=CARTESIAN_POINT('Origin',(-1.8357864376269,-3.9,21.4142135623731));
#18795=CARTESIAN_POINT('',(-2.00078643762691,-3.8,21.4142135623731));
#18796=CARTESIAN_POINT('Origin',(-1.8357864376269,-3.8,21.4142135623731));
#18797=CARTESIAN_POINT('',(-2.00078643762691,-2.2,21.4142135623731));
#18798=CARTESIAN_POINT('',(-2.00078643762691,-3.9,21.4142135623731));
#18799=CARTESIAN_POINT('Origin',(-1.8357864376269,-2.2,21.4142135623731));
#18800=CARTESIAN_POINT('Origin',(-1.83578643762691,-3.9,18.5857864376269));
#18801=CARTESIAN_POINT('',(-2.00078643762691,-3.8,18.5857864376269));
#18802=CARTESIAN_POINT('Origin',(-1.83578643762691,-3.8,18.5857864376269));
#18803=CARTESIAN_POINT('',(-2.00078643762691,-2.2,18.5857864376269));
#18804=CARTESIAN_POINT('',(-2.00078643762691,-3.9,18.5857864376269));
#18805=CARTESIAN_POINT('Origin',(-1.83578643762691,-2.2,18.5857864376269));
#18806=CARTESIAN_POINT('Origin',(-6.05,-3.,0.9));
#18807=CARTESIAN_POINT('',(-6.275,-3.,1.));
#18808=CARTESIAN_POINT('Origin',(-6.05,-3.,1.));
#18809=CARTESIAN_POINT('',(-6.275,-3.,1.8));
#18810=CARTESIAN_POINT('',(-6.275,-3.,0.9));
#18811=CARTESIAN_POINT('Origin',(-6.05,-3.,1.8));
#18812=CARTESIAN_POINT('Origin',(-0.45,-3.,0.9));
#18813=CARTESIAN_POINT('',(-0.675,-3.,1.));
#18814=CARTESIAN_POINT('Origin',(-0.45,-3.,1.));
#18815=CARTESIAN_POINT('',(-0.675,-3.,1.8));
#18816=CARTESIAN_POINT('',(-0.675,-3.,0.9));
#18817=CARTESIAN_POINT('Origin',(-0.45,-3.,1.8));
#18818=CARTESIAN_POINT('Origin',(-3.25,-3.9,20.));
#18819=CARTESIAN_POINT('',(-4.85,-3.8,20.));
#18820=CARTESIAN_POINT('Origin',(-3.25,-3.8,20.));
#18821=CARTESIAN_POINT('',(-4.85,-2.2,20.));
#18822=CARTESIAN_POINT('',(-4.85,-3.9,20.));
#18823=CARTESIAN_POINT('Origin',(-3.25,-2.2,20.));
#18824=CARTESIAN_POINT('Origin',(-6.65,-3.8,1.8));
#18825=CARTESIAN_POINT('',(-0.85,-3.8,1.8));
#18826=CARTESIAN_POINT('',(-0.85,-2.2,1.8));
#18827=CARTESIAN_POINT('',(-0.85,-3.8,1.8));
#18828=CARTESIAN_POINT('',(0.15,-3.8,1.8));
#18829=CARTESIAN_POINT('',(0.15,-3.8,1.8));
#18830=CARTESIAN_POINT('',(0.15,-2.2,1.8));
#18831=CARTESIAN_POINT('',(0.15,-3.8,1.8));
#18832=CARTESIAN_POINT('',(0.15,-2.2,1.8));
#18833=CARTESIAN_POINT('Origin',(-6.65,-3.8,1.8));
#18834=CARTESIAN_POINT('',(-5.65,-2.2,1.8));
#18835=CARTESIAN_POINT('',(-5.65,-3.8,1.8));
#18836=CARTESIAN_POINT('',(-5.65,-3.,1.8));
#18837=CARTESIAN_POINT('',(-6.65,-2.2,1.8));
#18838=CARTESIAN_POINT('',(0.15,-2.2,1.8));
#18839=CARTESIAN_POINT('',(-6.65,-3.8,1.8));
#18840=CARTESIAN_POINT('',(-6.65,-3.8,1.8));
#18841=CARTESIAN_POINT('',(0.15,-3.8,1.8));
#18842=CARTESIAN_POINT('Origin',(-6.65,-3.8,1.));
#18843=CARTESIAN_POINT('',(-6.65,-3.8,1.));
#18844=CARTESIAN_POINT('',(-6.65,-3.8,1.8));
#18845=CARTESIAN_POINT('',(-6.65,-2.2,1.));
#18846=CARTESIAN_POINT('',(-6.65,-2.2,1.8));
#18847=CARTESIAN_POINT('',(-6.65,-3.8,1.));
#18848=CARTESIAN_POINT('Origin',(0.15,-3.8,1.8));
#18849=CARTESIAN_POINT('',(0.15,-3.8,1.));
#18850=CARTESIAN_POINT('',(0.15,-3.8,1.));
#18851=CARTESIAN_POINT('',(0.15,-2.2,1.));
#18852=CARTESIAN_POINT('',(0.15,-3.8,1.));
#18853=CARTESIAN_POINT('',(0.15,-2.2,1.));
#18854=CARTESIAN_POINT('Origin',(-5.65,-3.8,1.));
#18855=CARTESIAN_POINT('',(-0.85,-3.8,22.5));
#18856=CARTESIAN_POINT('',(-0.85,-3.8,1.));
#18857=CARTESIAN_POINT('',(-5.65,-3.8,22.5));
#18858=CARTESIAN_POINT('',(-5.65,-3.8,22.5));
#18859=CARTESIAN_POINT('',(-5.65,-3.8,1.));
#18860=CARTESIAN_POINT('',(-6.65,-3.8,1.));
#18861=CARTESIAN_POINT('Origin',(-0.85,-3.8,1.));
#18862=CARTESIAN_POINT('',(-0.85,-2.2,22.5));
#18863=CARTESIAN_POINT('',(-0.85,-2.2,1.));
#18864=CARTESIAN_POINT('',(-0.85,-3.8,22.5));
#18865=CARTESIAN_POINT('Origin',(-0.85,-2.2,1.));
#18866=CARTESIAN_POINT('',(-5.65,-2.2,22.5));
#18867=CARTESIAN_POINT('',(-5.65,-2.2,1.));
#18868=CARTESIAN_POINT('',(-0.85,-2.2,22.5));
#18869=CARTESIAN_POINT('',(-6.65,-2.2,1.));
#18870=CARTESIAN_POINT('Origin',(-5.65,-2.2,1.));
#18871=CARTESIAN_POINT('',(-5.65,-2.2,22.5));
#18872=CARTESIAN_POINT('Origin',(-3.25,-3.,22.5));
#18873=CARTESIAN_POINT('Origin',(-3.25,-3.,1.));
#18874=CARTESIAN_POINT('',(0.,0.,0.));
#18875=CARTESIAN_POINT('Origin',(-4.66421356237309,-4.1,18.5857864376269));
#18876=CARTESIAN_POINT('',(-4.88921356237309,-4.,18.5857864376269));
#18877=CARTESIAN_POINT('Origin',(-4.66421356237309,-4.,18.5857864376269));
#18878=CARTESIAN_POINT('',(-4.88921356237309,-3.8,18.5857864376269));
#18879=CARTESIAN_POINT('',(-4.88921356237309,-4.1,18.5857864376269));
#18880=CARTESIAN_POINT('Origin',(-4.66421356237309,-3.8,18.5857864376269));
#18881=CARTESIAN_POINT('Origin',(-4.66421356237309,-4.1,21.4142135623731));
#18882=CARTESIAN_POINT('',(-4.88921356237309,-4.,21.4142135623731));
#18883=CARTESIAN_POINT('Origin',(-4.66421356237309,-4.,21.4142135623731));
#18884=CARTESIAN_POINT('',(-4.88921356237309,-3.8,21.4142135623731));
#18885=CARTESIAN_POINT('',(-4.88921356237309,-4.1,21.4142135623731));
#18886=CARTESIAN_POINT('Origin',(-4.66421356237309,-3.8,21.4142135623731));
#18887=CARTESIAN_POINT('Origin',(-1.8357864376269,-4.1,21.4142135623731));
#18888=CARTESIAN_POINT('',(-2.0607864376269,-4.,21.4142135623731));
#18889=CARTESIAN_POINT('Origin',(-1.8357864376269,-4.,21.4142135623731));
#18890=CARTESIAN_POINT('',(-2.0607864376269,-3.8,21.4142135623731));
#18891=CARTESIAN_POINT('',(-2.0607864376269,-4.1,21.4142135623731));
#18892=CARTESIAN_POINT('Origin',(-1.8357864376269,-3.8,21.4142135623731));
#18893=CARTESIAN_POINT('Origin',(-1.83578643762691,-4.1,18.5857864376269));
#18894=CARTESIAN_POINT('',(-2.06078643762691,-4.,18.5857864376269));
#18895=CARTESIAN_POINT('Origin',(-1.83578643762691,-4.,18.5857864376269));
#18896=CARTESIAN_POINT('',(-2.06078643762691,-3.8,18.5857864376269));
#18897=CARTESIAN_POINT('',(-2.06078643762691,-4.1,18.5857864376269));
#18898=CARTESIAN_POINT('Origin',(-1.83578643762691,-3.8,18.5857864376269));
#18899=CARTESIAN_POINT('Origin',(-3.25,-3.8,20.));
#18900=CARTESIAN_POINT('',(-4.84,-3.5,20.));
#18901=CARTESIAN_POINT('Origin',(-3.25,-3.5,20.));
#18902=CARTESIAN_POINT('',(-4.84,-3.8,20.));
#18903=CARTESIAN_POINT('',(-4.84,-3.8,20.));
#18904=CARTESIAN_POINT('Origin',(-3.25,-3.8,20.));
#18905=CARTESIAN_POINT('Origin',(-3.25,-3.5,20.));
#18906=CARTESIAN_POINT('',(-4.66,-3.5,20.));
#18907=CARTESIAN_POINT('Origin',(-3.25,-3.5,20.));
#18908=CARTESIAN_POINT('Origin',(-3.25,-4.,20.));
#18909=CARTESIAN_POINT('',(-4.66,-4.,20.));
#18910=CARTESIAN_POINT('',(-4.66,-4.,20.));
#18911=CARTESIAN_POINT('Origin',(-3.25,-4.,20.));
#18912=CARTESIAN_POINT('Origin',(-3.25,-4.,20.));
#18913=CARTESIAN_POINT('',(-5.65,-3.8,20.));
#18914=CARTESIAN_POINT('Origin',(-3.25,-3.8,20.));
#18915=CARTESIAN_POINT('',(-5.65,-4.,20.));
#18916=CARTESIAN_POINT('',(-5.65,-4.,20.));
#18917=CARTESIAN_POINT('Origin',(-3.25,-4.,20.));
#18918=CARTESIAN_POINT('Origin',(-3.25,-3.8,20.));
#18919=CARTESIAN_POINT('Origin',(-3.25,-4.,20.));
#18920=CARTESIAN_POINT('',(0.,0.,0.));
#18921=CARTESIAN_POINT('Origin',(-4.66421356237309,-2.3,18.5857864376269));
#18922=CARTESIAN_POINT('',(-4.88921356237309,-2.2,18.5857864376269));
#18923=CARTESIAN_POINT('Origin',(-4.66421356237309,-2.2,18.5857864376269));
#18924=CARTESIAN_POINT('',(-4.88921356237309,-2.,18.5857864376269));
#18925=CARTESIAN_POINT('',(-4.88921356237309,-2.3,18.5857864376269));
#18926=CARTESIAN_POINT('Origin',(-4.66421356237309,-2.,18.5857864376269));
#18927=CARTESIAN_POINT('Origin',(-4.66421356237309,-2.3,21.4142135623731));
#18928=CARTESIAN_POINT('',(-4.88921356237309,-2.2,21.4142135623731));
#18929=CARTESIAN_POINT('Origin',(-4.66421356237309,-2.2,21.4142135623731));
#18930=CARTESIAN_POINT('',(-4.88921356237309,-2.,21.4142135623731));
#18931=CARTESIAN_POINT('',(-4.88921356237309,-2.3,21.4142135623731));
#18932=CARTESIAN_POINT('Origin',(-4.66421356237309,-2.,21.4142135623731));
#18933=CARTESIAN_POINT('Origin',(-1.8357864376269,-2.3,21.4142135623731));
#18934=CARTESIAN_POINT('',(-2.0607864376269,-2.2,21.4142135623731));
#18935=CARTESIAN_POINT('Origin',(-1.8357864376269,-2.2,21.4142135623731));
#18936=CARTESIAN_POINT('',(-2.0607864376269,-2.,21.4142135623731));
#18937=CARTESIAN_POINT('',(-2.0607864376269,-2.3,21.4142135623731));
#18938=CARTESIAN_POINT('Origin',(-1.8357864376269,-2.,21.4142135623731));
#18939=CARTESIAN_POINT('Origin',(-1.83578643762691,-2.3,18.5857864376269));
#18940=CARTESIAN_POINT('',(-2.06078643762691,-2.2,18.5857864376269));
#18941=CARTESIAN_POINT('Origin',(-1.83578643762691,-2.2,18.5857864376269));
#18942=CARTESIAN_POINT('',(-2.06078643762691,-2.,18.5857864376269));
#18943=CARTESIAN_POINT('',(-2.06078643762691,-2.3,18.5857864376269));
#18944=CARTESIAN_POINT('Origin',(-1.83578643762691,-2.,18.5857864376269));
#18945=CARTESIAN_POINT('Origin',(-3.25,-2.5,20.));
#18946=CARTESIAN_POINT('',(-4.84,-2.2,20.));
#18947=CARTESIAN_POINT('Origin',(-3.25,-2.2,20.));
#18948=CARTESIAN_POINT('',(-4.84,-2.5,20.));
#18949=CARTESIAN_POINT('',(-4.84,-2.5,20.));
#18950=CARTESIAN_POINT('Origin',(-3.25,-2.5,20.));
#18951=CARTESIAN_POINT('Origin',(-3.25,-2.5,20.));
#18952=CARTESIAN_POINT('',(-4.66,-2.5,20.));
#18953=CARTESIAN_POINT('Origin',(-3.25,-2.5,20.));
#18954=CARTESIAN_POINT('Origin',(-3.25,-2.2,20.));
#18955=CARTESIAN_POINT('',(-4.66,-2.,20.));
#18956=CARTESIAN_POINT('Origin',(-3.25,-2.,20.));
#18957=CARTESIAN_POINT('',(-4.66,-2.2,20.));
#18958=CARTESIAN_POINT('Origin',(-3.25,-2.2,20.));
#18959=CARTESIAN_POINT('',(-5.65,-2.,20.));
#18960=CARTESIAN_POINT('Origin',(-3.25,-2.,20.));
#18961=CARTESIAN_POINT('',(-5.65,-2.2,20.));
#18962=CARTESIAN_POINT('',(-5.65,-2.2,20.));
#18963=CARTESIAN_POINT('Origin',(-3.25,-2.2,20.));
#18964=CARTESIAN_POINT('Origin',(-3.25,-2.,20.));
#18965=CARTESIAN_POINT('Origin',(-3.25,-2.2,20.));
#18966=CARTESIAN_POINT('',(0.,0.,0.));
#18967=CARTESIAN_POINT('Origin',(-4.66421356237309,2.1,18.5857864376269));
#18968=CARTESIAN_POINT('',(-4.82921356237309,2.2,18.5857864376269));
#18969=CARTESIAN_POINT('Origin',(-4.66421356237309,2.2,18.5857864376269));
#18970=CARTESIAN_POINT('',(-4.82921356237309,3.8,18.5857864376269));
#18971=CARTESIAN_POINT('',(-4.82921356237309,2.1,18.5857864376269));
#18972=CARTESIAN_POINT('Origin',(-4.66421356237309,3.8,18.5857864376269));
#18973=CARTESIAN_POINT('Origin',(-4.66421356237309,2.1,21.4142135623731));
#18974=CARTESIAN_POINT('',(-4.82921356237309,2.2,21.4142135623731));
#18975=CARTESIAN_POINT('Origin',(-4.66421356237309,2.2,21.4142135623731));
#18976=CARTESIAN_POINT('',(-4.82921356237309,3.8,21.4142135623731));
#18977=CARTESIAN_POINT('',(-4.82921356237309,2.1,21.4142135623731));
#18978=CARTESIAN_POINT('Origin',(-4.66421356237309,3.8,21.4142135623731));
#18979=CARTESIAN_POINT('Origin',(-1.8357864376269,2.1,21.4142135623731));
#18980=CARTESIAN_POINT('',(-2.00078643762691,2.2,21.4142135623731));
#18981=CARTESIAN_POINT('Origin',(-1.8357864376269,2.2,21.4142135623731));
#18982=CARTESIAN_POINT('',(-2.00078643762691,3.8,21.4142135623731));
#18983=CARTESIAN_POINT('',(-2.00078643762691,2.1,21.4142135623731));
#18984=CARTESIAN_POINT('Origin',(-1.8357864376269,3.8,21.4142135623731));
#18985=CARTESIAN_POINT('Origin',(-1.83578643762691,2.1,18.5857864376269));
#18986=CARTESIAN_POINT('',(-2.00078643762691,2.2,18.5857864376269));
#18987=CARTESIAN_POINT('Origin',(-1.83578643762691,2.2,18.5857864376269));
#18988=CARTESIAN_POINT('',(-2.00078643762691,3.8,18.5857864376269));
#18989=CARTESIAN_POINT('',(-2.00078643762691,2.1,18.5857864376269));
#18990=CARTESIAN_POINT('Origin',(-1.83578643762691,3.8,18.5857864376269));
#18991=CARTESIAN_POINT('Origin',(-6.05,3.,0.9));
#18992=CARTESIAN_POINT('',(-6.275,3.,1.));
#18993=CARTESIAN_POINT('Origin',(-6.05,3.,1.));
#18994=CARTESIAN_POINT('',(-6.275,3.,1.8));
#18995=CARTESIAN_POINT('',(-6.275,3.,0.9));
#18996=CARTESIAN_POINT('Origin',(-6.05,3.,1.8));
#18997=CARTESIAN_POINT('Origin',(-0.45,3.,0.9));
#18998=CARTESIAN_POINT('',(-0.675,3.,1.));
#18999=CARTESIAN_POINT('Origin',(-0.45,3.,1.));
#19000=CARTESIAN_POINT('',(-0.675,3.,1.8));
#19001=CARTESIAN_POINT('',(-0.675,3.,0.9));
#19002=CARTESIAN_POINT('Origin',(-0.45,3.,1.8));
#19003=CARTESIAN_POINT('Origin',(-3.25,2.1,20.));
#19004=CARTESIAN_POINT('',(-4.85,2.2,20.));
#19005=CARTESIAN_POINT('Origin',(-3.25,2.2,20.));
#19006=CARTESIAN_POINT('',(-4.85,3.8,20.));
#19007=CARTESIAN_POINT('',(-4.85,2.1,20.));
#19008=CARTESIAN_POINT('Origin',(-3.25,3.8,20.));
#19009=CARTESIAN_POINT('Origin',(-6.65,2.2,1.8));
#19010=CARTESIAN_POINT('',(-0.85,2.2,1.8));
#19011=CARTESIAN_POINT('',(-0.85,3.8,1.8));
#19012=CARTESIAN_POINT('',(-0.85,2.2,1.8));
#19013=CARTESIAN_POINT('',(0.15,2.2,1.8));
#19014=CARTESIAN_POINT('',(0.15,2.2,1.8));
#19015=CARTESIAN_POINT('',(0.15,3.8,1.8));
#19016=CARTESIAN_POINT('',(0.15,2.2,1.8));
#19017=CARTESIAN_POINT('',(0.15,3.8,1.8));
#19018=CARTESIAN_POINT('Origin',(-6.65,2.2,1.8));
#19019=CARTESIAN_POINT('',(-5.65,3.8,1.8));
#19020=CARTESIAN_POINT('',(-5.65,2.2,1.8));
#19021=CARTESIAN_POINT('',(-5.65,3.,1.8));
#19022=CARTESIAN_POINT('',(-6.65,3.8,1.8));
#19023=CARTESIAN_POINT('',(0.15,3.8,1.8));
#19024=CARTESIAN_POINT('',(-6.65,2.2,1.8));
#19025=CARTESIAN_POINT('',(-6.65,2.2,1.8));
#19026=CARTESIAN_POINT('',(0.15,2.2,1.8));
#19027=CARTESIAN_POINT('Origin',(-6.65,2.2,1.));
#19028=CARTESIAN_POINT('',(-6.65,2.2,1.));
#19029=CARTESIAN_POINT('',(-6.65,2.2,1.8));
#19030=CARTESIAN_POINT('',(-6.65,3.8,1.));
#19031=CARTESIAN_POINT('',(-6.65,3.8,1.8));
#19032=CARTESIAN_POINT('',(-6.65,2.2,1.));
#19033=CARTESIAN_POINT('Origin',(0.15,2.2,1.8));
#19034=CARTESIAN_POINT('',(0.15,2.2,1.));
#19035=CARTESIAN_POINT('',(0.15,2.2,1.));
#19036=CARTESIAN_POINT('',(0.15,3.8,1.));
#19037=CARTESIAN_POINT('',(0.15,2.2,1.));
#19038=CARTESIAN_POINT('',(0.15,3.8,1.));
#19039=CARTESIAN_POINT('Origin',(-5.65,2.2,1.));
#19040=CARTESIAN_POINT('',(-0.85,2.2,22.5));
#19041=CARTESIAN_POINT('',(-0.85,2.2,1.));
#19042=CARTESIAN_POINT('',(-5.65,2.2,22.5));
#19043=CARTESIAN_POINT('',(-5.65,2.2,22.5));
#19044=CARTESIAN_POINT('',(-5.65,2.2,1.));
#19045=CARTESIAN_POINT('',(-6.65,2.2,1.));
#19046=CARTESIAN_POINT('Origin',(-0.85,2.2,1.));
#19047=CARTESIAN_POINT('',(-0.85,3.8,22.5));
#19048=CARTESIAN_POINT('',(-0.85,3.8,1.));
#19049=CARTESIAN_POINT('',(-0.85,2.2,22.5));
#19050=CARTESIAN_POINT('Origin',(-0.85,3.8,1.));
#19051=CARTESIAN_POINT('',(-5.65,3.8,22.5));
#19052=CARTESIAN_POINT('',(-5.65,3.8,1.));
#19053=CARTESIAN_POINT('',(-0.85,3.8,22.5));
#19054=CARTESIAN_POINT('',(-6.65,3.8,1.));
#19055=CARTESIAN_POINT('Origin',(-5.65,3.8,1.));
#19056=CARTESIAN_POINT('',(-5.65,3.8,22.5));
#19057=CARTESIAN_POINT('Origin',(-3.25,3.,22.5));
#19058=CARTESIAN_POINT('Origin',(-3.25,3.,1.));
#19059=CARTESIAN_POINT('',(0.,0.,0.));
#19060=CARTESIAN_POINT('Origin',(-4.66421356237309,1.9,18.5857864376269));
#19061=CARTESIAN_POINT('',(-4.88921356237309,2.,18.5857864376269));
#19062=CARTESIAN_POINT('Origin',(-4.66421356237309,2.,18.5857864376269));
#19063=CARTESIAN_POINT('',(-4.88921356237309,2.2,18.5857864376269));
#19064=CARTESIAN_POINT('',(-4.88921356237309,1.9,18.5857864376269));
#19065=CARTESIAN_POINT('Origin',(-4.66421356237309,2.2,18.5857864376269));
#19066=CARTESIAN_POINT('Origin',(-4.66421356237309,1.9,21.4142135623731));
#19067=CARTESIAN_POINT('',(-4.88921356237309,2.,21.4142135623731));
#19068=CARTESIAN_POINT('Origin',(-4.66421356237309,2.,21.4142135623731));
#19069=CARTESIAN_POINT('',(-4.88921356237309,2.2,21.4142135623731));
#19070=CARTESIAN_POINT('',(-4.88921356237309,1.9,21.4142135623731));
#19071=CARTESIAN_POINT('Origin',(-4.66421356237309,2.2,21.4142135623731));
#19072=CARTESIAN_POINT('Origin',(-1.8357864376269,1.9,21.4142135623731));
#19073=CARTESIAN_POINT('',(-2.0607864376269,2.,21.4142135623731));
#19074=CARTESIAN_POINT('Origin',(-1.8357864376269,2.,21.4142135623731));
#19075=CARTESIAN_POINT('',(-2.0607864376269,2.2,21.4142135623731));
#19076=CARTESIAN_POINT('',(-2.0607864376269,1.9,21.4142135623731));
#19077=CARTESIAN_POINT('Origin',(-1.8357864376269,2.2,21.4142135623731));
#19078=CARTESIAN_POINT('Origin',(-1.83578643762691,1.9,18.5857864376269));
#19079=CARTESIAN_POINT('',(-2.06078643762691,2.,18.5857864376269));
#19080=CARTESIAN_POINT('Origin',(-1.83578643762691,2.,18.5857864376269));
#19081=CARTESIAN_POINT('',(-2.06078643762691,2.2,18.5857864376269));
#19082=CARTESIAN_POINT('',(-2.06078643762691,1.9,18.5857864376269));
#19083=CARTESIAN_POINT('Origin',(-1.83578643762691,2.2,18.5857864376269));
#19084=CARTESIAN_POINT('Origin',(-3.25,2.2,20.));
#19085=CARTESIAN_POINT('',(-4.84,2.5,20.));
#19086=CARTESIAN_POINT('Origin',(-3.25,2.5,20.));
#19087=CARTESIAN_POINT('',(-4.84,2.2,20.));
#19088=CARTESIAN_POINT('',(-4.84,2.2,20.));
#19089=CARTESIAN_POINT('Origin',(-3.25,2.2,20.));
#19090=CARTESIAN_POINT('Origin',(-3.25,2.5,20.));
#19091=CARTESIAN_POINT('',(-4.66,2.5,20.));
#19092=CARTESIAN_POINT('Origin',(-3.25,2.5,20.));
#19093=CARTESIAN_POINT('Origin',(-3.25,2.,20.));
#19094=CARTESIAN_POINT('',(-4.66,2.,20.));
#19095=CARTESIAN_POINT('',(-4.66,2.,20.));
#19096=CARTESIAN_POINT('Origin',(-3.25,2.,20.));
#19097=CARTESIAN_POINT('Origin',(-3.25,2.,20.));
#19098=CARTESIAN_POINT('',(-5.65,2.2,20.));
#19099=CARTESIAN_POINT('Origin',(-3.25,2.2,20.));
#19100=CARTESIAN_POINT('',(-5.65,2.,20.));
#19101=CARTESIAN_POINT('',(-5.65,2.,20.));
#19102=CARTESIAN_POINT('Origin',(-3.25,2.,20.));
#19103=CARTESIAN_POINT('Origin',(-3.25,2.2,20.));
#19104=CARTESIAN_POINT('Origin',(-3.25,2.,20.));
#19105=CARTESIAN_POINT('',(0.,0.,0.));
#19106=CARTESIAN_POINT('Origin',(-4.66421356237309,3.7,18.5857864376269));
#19107=CARTESIAN_POINT('',(-4.88921356237309,3.8,18.5857864376269));
#19108=CARTESIAN_POINT('Origin',(-4.66421356237309,3.8,18.5857864376269));
#19109=CARTESIAN_POINT('',(-4.88921356237309,4.,18.5857864376269));
#19110=CARTESIAN_POINT('',(-4.88921356237309,3.7,18.5857864376269));
#19111=CARTESIAN_POINT('Origin',(-4.66421356237309,4.,18.5857864376269));
#19112=CARTESIAN_POINT('Origin',(-4.66421356237309,3.7,21.4142135623731));
#19113=CARTESIAN_POINT('',(-4.88921356237309,3.8,21.4142135623731));
#19114=CARTESIAN_POINT('Origin',(-4.66421356237309,3.8,21.4142135623731));
#19115=CARTESIAN_POINT('',(-4.88921356237309,4.,21.4142135623731));
#19116=CARTESIAN_POINT('',(-4.88921356237309,3.7,21.4142135623731));
#19117=CARTESIAN_POINT('Origin',(-4.66421356237309,4.,21.4142135623731));
#19118=CARTESIAN_POINT('Origin',(-1.8357864376269,3.7,21.4142135623731));
#19119=CARTESIAN_POINT('',(-2.0607864376269,3.8,21.4142135623731));
#19120=CARTESIAN_POINT('Origin',(-1.8357864376269,3.8,21.4142135623731));
#19121=CARTESIAN_POINT('',(-2.0607864376269,4.,21.4142135623731));
#19122=CARTESIAN_POINT('',(-2.0607864376269,3.7,21.4142135623731));
#19123=CARTESIAN_POINT('Origin',(-1.8357864376269,4.,21.4142135623731));
#19124=CARTESIAN_POINT('Origin',(-1.83578643762691,3.7,18.5857864376269));
#19125=CARTESIAN_POINT('',(-2.06078643762691,3.8,18.5857864376269));
#19126=CARTESIAN_POINT('Origin',(-1.83578643762691,3.8,18.5857864376269));
#19127=CARTESIAN_POINT('',(-2.06078643762691,4.,18.5857864376269));
#19128=CARTESIAN_POINT('',(-2.06078643762691,3.7,18.5857864376269));
#19129=CARTESIAN_POINT('Origin',(-1.83578643762691,4.,18.5857864376269));
#19130=CARTESIAN_POINT('Origin',(-3.25,3.5,20.));
#19131=CARTESIAN_POINT('',(-4.84,3.8,20.));
#19132=CARTESIAN_POINT('Origin',(-3.25,3.8,20.));
#19133=CARTESIAN_POINT('',(-4.84,3.5,20.));
#19134=CARTESIAN_POINT('',(-4.84,3.5,20.));
#19135=CARTESIAN_POINT('Origin',(-3.25,3.5,20.));
#19136=CARTESIAN_POINT('Origin',(-3.25,3.5,20.));
#19137=CARTESIAN_POINT('',(-4.66,3.5,20.));
#19138=CARTESIAN_POINT('Origin',(-3.25,3.5,20.));
#19139=CARTESIAN_POINT('Origin',(-3.25,3.8,20.));
#19140=CARTESIAN_POINT('',(-4.66,4.,20.));
#19141=CARTESIAN_POINT('Origin',(-3.25,4.,20.));
#19142=CARTESIAN_POINT('',(-4.66,3.8,20.));
#19143=CARTESIAN_POINT('Origin',(-3.25,3.8,20.));
#19144=CARTESIAN_POINT('',(-5.65,4.,20.));
#19145=CARTESIAN_POINT('Origin',(-3.25,4.,20.));
#19146=CARTESIAN_POINT('',(-5.65,3.8,20.));
#19147=CARTESIAN_POINT('',(-5.65,3.8,20.));
#19148=CARTESIAN_POINT('Origin',(-3.25,3.8,20.));
#19149=CARTESIAN_POINT('Origin',(-3.25,4.,20.));
#19150=CARTESIAN_POINT('Origin',(-3.25,3.8,20.));
#19151=CARTESIAN_POINT('',(0.,0.,0.));
#19152=CARTESIAN_POINT('Origin',(12.,0.,0.));
#19153=CARTESIAN_POINT('',(12.,7.34788079488412E-17,0.6));
#19154=CARTESIAN_POINT('Origin',(12.,0.,0.));
#19155=CARTESIAN_POINT('Origin',(0.05,0.,0.));
#19156=CARTESIAN_POINT('',(0.1,7.34788079488412E-17,0.6));
#19157=CARTESIAN_POINT('Origin',(0.1,0.,0.));
#19158=CARTESIAN_POINT('',(0.,-6.12323399573677E-17,0.5));
#19159=CARTESIAN_POINT('',(0.05,-6.73555739531044E-17,0.55));
#19160=CARTESIAN_POINT('Origin',(0.,0.,0.));
#19161=CARTESIAN_POINT('Origin',(0.,0.,0.));
#19162=CARTESIAN_POINT('',(0.,-7.34788079488412E-17,0.6));
#19163=CARTESIAN_POINT('Origin',(0.,0.,0.));
#19164=CARTESIAN_POINT('',(0.,0.,0.));
#19165=CARTESIAN_POINT('',(0.,0.,0.));
#19166=CARTESIAN_POINT('Origin',(0.,0.,0.));
#19167=CARTESIAN_POINT('',(-1.070235,-0.308121667383195,-1.31065986708547E-16));
#19168=CARTESIAN_POINT('',(-1.31065986708547E-16,-0.308121667383195,1.070235));
#19169=CARTESIAN_POINT('Origin',(0.,-0.308121667383195,0.));
#19170=CARTESIAN_POINT('Origin',(0.,-0.308121667383195,0.));
#19171=CARTESIAN_POINT('',(-1.31065986708547E-16,0.308121667383195,1.070235));
#19172=CARTESIAN_POINT('Origin',(-1.34711147906209E-16,0.,1.1));
#19173=CARTESIAN_POINT('',(-1.070235,0.308121667383195,1.31065986708547E-16));
#19174=CARTESIAN_POINT('Origin',(0.,0.308121667383195,0.));
#19175=CARTESIAN_POINT('Origin',(0.,0.308121667383195,0.));
#19176=CARTESIAN_POINT('Origin',(0.,0.,0.));
#19177=CARTESIAN_POINT('',(-1.070235,0.5,-1.31065986708547E-16));
#19178=CARTESIAN_POINT('',(-1.070235,0.,-1.31065986708547E-16));
#19179=CARTESIAN_POINT('Origin',(0.,0.5,0.));
#19180=CARTESIAN_POINT('Origin',(0.,0.,0.));
#19181=CARTESIAN_POINT('',(-0.6,-0.44,-7.34788079488412E-17));
#19182=CARTESIAN_POINT('Origin',(0.,-0.44,0.));
#19183=CARTESIAN_POINT('',(-0.6,0.44,-7.34788079488412E-17));
#19184=CARTESIAN_POINT('',(-0.6,0.,-7.34788079488412E-17));
#19185=CARTESIAN_POINT('Origin',(0.,0.44,0.));
#19186=CARTESIAN_POINT('Origin',(0.,0.47,0.));
#19187=CARTESIAN_POINT('',(-0.66,0.5,-8.08266887437253E-17));
#19188=CARTESIAN_POINT('',(-0.63,0.47,-7.71527483462832E-17));
#19189=CARTESIAN_POINT('Origin',(0.,0.5,0.));
#19190=CARTESIAN_POINT('Origin',(1.070235,0.5,0.));
#19191=CARTESIAN_POINT('Origin',(0.,0.,0.));
#19192=CARTESIAN_POINT('',(-1.070235,-0.5,-1.31065986708547E-16));
#19193=CARTESIAN_POINT('Origin',(0.,-0.5,0.));
#19194=CARTESIAN_POINT('',(-1.070235,0.,-1.31065986708547E-16));
#19195=CARTESIAN_POINT('Origin',(0.66,-0.5,0.));
#19196=CARTESIAN_POINT('',(-0.66,-0.5,-8.08266887437253E-17));
#19197=CARTESIAN_POINT('Origin',(0.,-0.5,0.));
#19198=CARTESIAN_POINT('Origin',(0.,-0.47,0.));
#19199=CARTESIAN_POINT('',(-0.63,-0.47,-7.71527483462832E-17));
#19200=CARTESIAN_POINT('',(0.,0.,0.));
#19201=CARTESIAN_POINT('Origin',(0.,0.,0.));
#19202=CARTESIAN_POINT('',(-1.129765,0.308121667383195,-1.38356309103871E-16));
#19203=CARTESIAN_POINT('',(-1.38356309103871E-16,0.308121667383195,1.129765));
#19204=CARTESIAN_POINT('Origin',(0.,0.308121667383195,0.));
#19205=CARTESIAN_POINT('Origin',(0.,0.308121667383195,0.));
#19206=CARTESIAN_POINT('',(-1.38356309103871E-16,-0.308121667383195,1.129765));
#19207=CARTESIAN_POINT('Origin',(-1.34711147906209E-16,0.,1.1));
#19208=CARTESIAN_POINT('',(-1.129765,-0.308121667383195,1.38356309103871E-16));
#19209=CARTESIAN_POINT('Origin',(0.,-0.308121667383195,0.));
#19210=CARTESIAN_POINT('Origin',(0.,-0.308121667383195,0.));
#19211=CARTESIAN_POINT('Origin',(0.,0.,0.));
#19212=CARTESIAN_POINT('',(-1.129765,-0.5,-1.38356309103871E-16));
#19213=CARTESIAN_POINT('Origin',(0.,-0.5,0.));
#19214=CARTESIAN_POINT('',(-1.129765,0.,-1.38356309103871E-16));
#19215=CARTESIAN_POINT('Origin',(1.54,0.5,0.));
#19216=CARTESIAN_POINT('',(-1.54,0.5,-1.88595607068692E-16));
#19217=CARTESIAN_POINT('Origin',(0.,0.5,0.));
#19218=CARTESIAN_POINT('',(-1.129765,0.5,-1.38356309103871E-16));
#19219=CARTESIAN_POINT('Origin',(0.,0.5,0.));
#19220=CARTESIAN_POINT('Origin',(0.,0.47,0.));
#19221=CARTESIAN_POINT('',(-1.6,0.44,-1.95943487863577E-16));
#19222=CARTESIAN_POINT('Origin',(0.,0.44,0.));
#19223=CARTESIAN_POINT('',(-1.57,0.47,-1.92269547466134E-16));
#19224=CARTESIAN_POINT('Origin',(0.,0.,0.));
#19225=CARTESIAN_POINT('',(-1.6,-0.44,-1.95943487863577E-16));
#19226=CARTESIAN_POINT('Origin',(0.,-0.44,0.));
#19227=CARTESIAN_POINT('',(-1.6,0.,-1.95943487863577E-16));
#19228=CARTESIAN_POINT('Origin',(0.,-0.47,0.));
#19229=CARTESIAN_POINT('',(-1.54,-0.5,-1.88595607068692E-16));
#19230=CARTESIAN_POINT('Origin',(0.,-0.5,0.));
#19231=CARTESIAN_POINT('',(-1.57,-0.47,-1.92269547466134E-16));
#19232=CARTESIAN_POINT('Origin',(1.129765,-0.5,0.));
#19233=CARTESIAN_POINT('Origin',(0.,0.,0.));
#19234=CARTESIAN_POINT('',(-1.129765,0.,-1.38356309103871E-16));
#19235=CARTESIAN_POINT('',(0.,0.,0.));
#19236=CARTESIAN_POINT('Origin',(1.1,0.,0.));
#19237=CARTESIAN_POINT('',(1.1,-2.23201749654651E-33,0.29765));
#19238=CARTESIAN_POINT('',(1.1,-2.23201749654651E-33,-0.29765));
#19239=CARTESIAN_POINT('Origin',(1.1,0.,0.));
#19240=CARTESIAN_POINT('Origin',(0.685838782044607,0.,-0.860014630714833));
#19241=CARTESIAN_POINT('',(0.918550922801216,-5.31350540756609E-33,-0.674432891191581));
#19242=CARTESIAN_POINT('',(0.453126641287998,8.49470414473068E-34,-1.04559637023808));
#19243=CARTESIAN_POINT('Origin',(0.685838782044607,0.,-0.860014630714833));
#19244=CARTESIAN_POINT('Origin',(-0.244773027351946,0.,-1.07242070340001));
#19245=CARTESIAN_POINT('',(0.0454142657089739,-2.23201749654651E-33,-1.1386540593921));
#19246=CARTESIAN_POINT('',(-0.534960320412865,-2.23201749654651E-33,-1.00618734740791));
#19247=CARTESIAN_POINT('Origin',(-0.244773027351946,0.,-1.07242070340001));
#19248=CARTESIAN_POINT('Origin',(-0.991065754692661,0.,-0.477272113029314));
#19249=CARTESIAN_POINT('',(-0.86192025974432,8.49470414473067E-34,-0.745445496560469));
#19250=CARTESIAN_POINT('',(-1.120211249641,-5.31350540756609E-33,-0.209098729498159));
#19251=CARTESIAN_POINT('Origin',(-0.991065754692661,0.,-0.477272113029314));
#19252=CARTESIAN_POINT('Origin',(-0.991065754692661,0.,0.477272113029314));
#19253=CARTESIAN_POINT('',(-1.120211249641,-2.23201749654651E-33,0.209098729498159));
#19254=CARTESIAN_POINT('',(-0.86192025974432,-2.23201749654651E-33,0.745445496560469));
#19255=CARTESIAN_POINT('Origin',(-0.991065754692661,0.,0.477272113029314));
#19256=CARTESIAN_POINT('Origin',(-0.244773027351946,0.,1.07242070340001));
#19257=CARTESIAN_POINT('',(-0.534960320412866,-2.23201749654651E-33,1.00618734740791));
#19258=CARTESIAN_POINT('',(0.0454142657089737,-2.23201749654651E-33,1.1386540593921));
#19259=CARTESIAN_POINT('Origin',(-0.244773027351946,0.,1.07242070340001));
#19260=CARTESIAN_POINT('Origin',(0.685838782044607,0.,0.860014630714833));
#19261=CARTESIAN_POINT('',(0.453126641287998,-2.23201749654651E-33,1.04559637023808));
#19262=CARTESIAN_POINT('',(0.918550922801216,-2.23201749654651E-33,0.674432891191581));
#19263=CARTESIAN_POINT('Origin',(0.685838782044607,0.,0.860014630714833));
#19264=CARTESIAN_POINT('',(0.,0.,0.));
#19265=CARTESIAN_POINT('Origin',(0.685838782044607,0.,0.860014630714833));
#19266=CARTESIAN_POINT('',(0.413083465285518,-0.05953,0.993751811093549));
#19267=CARTESIAN_POINT('',(0.876916659919095,-0.05953,0.623857181492959));
#19268=CARTESIAN_POINT('Ctrl Pts',(0.413083465285518,-0.05953,0.993751811093549));
#19269=CARTESIAN_POINT('Ctrl Pts',(0.419070565453383,-0.0925528133349865,
0.991263089003441));
#19270=CARTESIAN_POINT('Ctrl Pts',(0.430199341854858,-0.124911173756694,
0.986608710139579));
#19271=CARTESIAN_POINT('Ctrl Pts',(0.457978755888596,-0.177924977804098,
0.973971221090534));
#19272=CARTESIAN_POINT('Ctrl Pts',(0.473077587363685,-0.199697230012983,
0.966820759530997));
#19273=CARTESIAN_POINT('Ctrl Pts',(0.507057380724533,-0.237895043532788,
0.949440676105255));
#19274=CARTESIAN_POINT('Ctrl Pts',(0.525933334162555,-0.254319232363049,
0.939198248544428));
#19275=CARTESIAN_POINT('Ctrl Pts',(0.564362943424238,-0.28018331644634,
0.916597376014514));
#19276=CARTESIAN_POINT('Ctrl Pts',(0.585840553788742,-0.29104845371857,
0.903141581680914));
#19277=CARTESIAN_POINT('Ctrl Pts',(0.629305439856167,-0.30527573347708,
0.873412008702649));
#19278=CARTESIAN_POINT('Ctrl Pts',(0.651278921914856,-0.308638795020976,
0.857118508332695));
#19279=CARTESIAN_POINT('Ctrl Pts',(0.690705563850638,-0.308638795020976,
0.825676810575914));
#19280=CARTESIAN_POINT('Ctrl Pts',(0.711480111898423,-0.30527573347708,
0.807879894508811));
#19281=CARTESIAN_POINT('Ctrl Pts',(0.750136149454208,-0.29104845371857,
0.772120216227122));
#19282=CARTESIAN_POINT('Ctrl Pts',(0.768033796848072,-0.28018331644634,
0.754175290318038));
#19283=CARTESIAN_POINT('Ctrl Pts',(0.798619410861634,-0.254319232363049,
0.721738358858166));
#19284=CARTESIAN_POINT('Ctrl Pts',(0.812805334167529,-0.237895043532788,
0.705614819529209));
#19285=CARTESIAN_POINT('Ctrl Pts',(0.837310877969633,-0.199697230012983,
0.676354402927683));
#19286=CARTESIAN_POINT('Ctrl Pts',(0.847641868610495,-0.177924977804098,
0.663225258065736));
#19287=CARTESIAN_POINT('Ctrl Pts',(0.866144010579847,-0.124911173756694,
0.638954437806245));
#19288=CARTESIAN_POINT('Ctrl Pts',(0.873158080166742,-0.0925528133349865,
0.62914037979579));
#19289=CARTESIAN_POINT('Ctrl Pts',(0.876916659919095,-0.05953,0.623857181492959));
#19290=CARTESIAN_POINT('',(0.437601487681057,-0.05953,1.03511272300331));
#19291=CARTESIAN_POINT('Origin',(0.685838782044607,-0.05953,0.860014630714833));
#19292=CARTESIAN_POINT('',(0.911784794170997,-0.05953,0.656964154625313));
#19293=CARTESIAN_POINT('Ctrl Pts',(0.911784794170998,-0.0595300000000001,
0.656964154625312));
#19294=CARTESIAN_POINT('Ctrl Pts',(0.909827729890942,-0.0762225747374255,
0.659680317203144));
#19295=CARTESIAN_POINT('Ctrl Pts',(0.907004864562642,-0.0928409665394228,
0.663576540841106));
#19296=CARTESIAN_POINT('Ctrl Pts',(0.895234408667242,-0.144299303100741,
0.679480524217551));
#19297=CARTESIAN_POINT('Ctrl Pts',(0.882797231409153,-0.177024326825049,
0.695831250979106));
#19298=CARTESIAN_POINT('Ctrl Pts',(0.854332839576145,-0.227269801620064,
0.73042219438957));
#19299=CARTESIAN_POINT('Ctrl Pts',(0.834863020612702,-0.251265615809407,
0.752807465209441));
#19300=CARTESIAN_POINT('Ctrl Pts',(0.800439809856111,-0.279889827963178,
0.789147407129766));
#19301=CARTESIAN_POINT('Ctrl Pts',(0.781998747691871,-0.290879136862659,
0.80756613568454));
#19302=CARTESIAN_POINT('Ctrl Pts',(0.742239891936898,-0.305251990234487,
0.844254137480382));
#19303=CARTESIAN_POINT('Ctrl Pts',(0.720906778729541,-0.308638795020976,
0.862505527716294));
#19304=CARTESIAN_POINT('Ctrl Pts',(0.680463863683392,-0.308638795020976,
0.894757676234429));
#19305=CARTESIAN_POINT('Ctrl Pts',(0.657923009631182,-0.305251990234488,
0.91149460735272));
#19306=CARTESIAN_POINT('Ctrl Pts',(0.613307674922609,-0.290879136862659,
0.942092777160053));
#19307=CARTESIAN_POINT('Ctrl Pts',(0.591247219971725,-0.279889827963178,
0.955972930713954));
#19308=CARTESIAN_POINT('Ctrl Pts',(0.548158511259202,-0.251265615809407,
0.981446681891443));
#19309=CARTESIAN_POINT('Ctrl Pts',(0.522002043615455,-0.227269801620063,
0.995447160474328));
#19310=CARTESIAN_POINT('Ctrl Pts',(0.481944444320713,-0.177024326825049,
1.01550068154148));
#19311=CARTESIAN_POINT('Ctrl Pts',(0.463236132117164,-0.14429930310074,
1.0239876538093));
#19312=CARTESIAN_POINT('Ctrl Pts',(0.445111721969657,-0.0928409665394226,
1.03192403056628));
#19313=CARTESIAN_POINT('Ctrl Pts',(0.440685038163619,-0.0762225747374254,
1.03380912944435));
#19314=CARTESIAN_POINT('Ctrl Pts',(0.437601487681056,-0.05953,1.03511272300331));
#19315=CARTESIAN_POINT('Origin',(0.685838782044607,-0.05953,0.860014630714833));
#19316=CARTESIAN_POINT('Origin',(0.,-0.208355,0.));
#19317=CARTESIAN_POINT('',(0.0548532617164168,-0.05953,1.12247250791415));
#19318=CARTESIAN_POINT('Origin',(0.,-0.05953,0.));
#19319=CARTESIAN_POINT('',(-0.536443649899848,-0.05953,0.987512846410683));
#19320=CARTESIAN_POINT('Ctrl Pts',(0.0548532617164173,-0.0595300000000001,
1.12247250791414));
#19321=CARTESIAN_POINT('Ctrl Pts',(0.05150947068137,-0.0762225747374254,
1.12263591311425));
#19322=CARTESIAN_POINT('Ctrl Pts',(0.0467032526342597,-0.0928409665394227,
1.12285816383385));
#19323=CARTESIAN_POINT('Ctrl Pts',(0.0269302585198975,-0.144299303100741,
1.12357162229597));
#19324=CARTESIAN_POINT('Ctrl Pts',(0.006392292392153,-0.177024326825049,
1.12404235695137));
#19325=CARTESIAN_POINT('Ctrl Pts',(-0.0383992541984087,-0.227269801620063,
1.12335509974011));
#19326=CARTESIAN_POINT('Ctrl Pts',(-0.0680399972366993,-0.251265615809407,
1.12208997038458));
#19327=CARTESIAN_POINT('Ctrl Pts',(-0.117914228755037,-0.279889827963178,
1.1178344036749));
#19328=CARTESIAN_POINT('Ctrl Pts',(-0.14381238480104,-0.290879136862659,
1.11490049012186));
#19329=CARTESIAN_POINT('Ctrl Pts',(-0.19728546073067,-0.305251990234488,
1.10669035995599));
#19330=CARTESIAN_POINT('Ctrl Pts',(-0.224855950742601,-0.308638795020976,
1.10139101611326));
#19331=CARTESIAN_POINT('Ctrl Pts',(-0.275287440920027,-0.308638795020976,
1.0898803575765));
#19332=CARTESIAN_POINT('Ctrl Pts',(-0.302426893214945,-0.305251990234488,
1.08269251410343));
#19333=CARTESIAN_POINT('Ctrl Pts',(-0.35416671187353,-0.290879136862659,
1.06688848765783));
#19334=CARTESIAN_POINT('Ctrl Pts',(-0.3787731215897,-0.279889827963178,
1.05829506364875));
#19335=CARTESIAN_POINT('Ctrl Pts',(-0.425554672694338,-0.251265615809407,
1.04048957871266));
#19336=CARTESIAN_POINT('Ctrl Pts',(-0.452808978448581,-0.227269801620063,
1.02876878445619));
#19337=CARTESIAN_POINT('Ctrl Pts',(-0.493462957200432,-0.177024326825049,
1.0099536580922));
#19338=CARTESIAN_POINT('Ctrl Pts',(-0.511762781179148,-0.14429930310074,
1.00061845128527));
#19339=CARTESIAN_POINT('Ctrl Pts',(-0.529268075276157,-0.0928409665394226,
0.991396466802468));
#19340=CARTESIAN_POINT('Ctrl Pts',(-0.533501897135713,-0.0762225747374254,
0.989110885965947));
#19341=CARTESIAN_POINT('Ctrl Pts',(-0.536443649899848,-0.0595300000000001,
0.987512846410683));
#19342=CARTESIAN_POINT('',(-0.843383895613249,-0.05953,0.742736168477219));
#19343=CARTESIAN_POINT('Origin',(0.,-0.05953,0.));
#19344=CARTESIAN_POINT('',(-1.10653577764992,-0.05953,0.196295654879792));
#19345=CARTESIAN_POINT('Ctrl Pts',(-0.843383895613249,-0.0595300000000001,
0.742736168477219));
#19346=CARTESIAN_POINT('Ctrl Pts',(-0.84559647055299,-0.0762225747374255,
0.740223768851062));
#19347=CARTESIAN_POINT('Ctrl Pts',(-0.848766861100456,-0.0928409665394227,
0.736604687327351));
#19348=CARTESIAN_POINT('Ctrl Pts',(-0.861652925570091,-0.144299303100741,
0.721590372101268));
#19349=CARTESIAN_POINT('Ctrl Pts',(-0.87482617317514,-0.177024326825049,
0.705826641853758));
#19350=CARTESIAN_POINT('Ctrl Pts',(-0.902215926359523,-0.227269801620063,
0.670378702718353));
#19351=CARTESIAN_POINT('Ctrl Pts',(-0.919707509403859,-0.251265615809407,
0.646415841396062));
#19352=CARTESIAN_POINT('Ctrl Pts',(-0.947476448101718,-0.279889827963178,
0.604769294586516));
#19353=CARTESIAN_POINT('Ctrl Pts',(-0.961329858300736,-0.290879136862659,
0.582692035672022));
#19354=CARTESIAN_POINT('Ctrl Pts',(-0.988250837578047,-0.305251990234488,
0.535766169015486));
#19355=CARTESIAN_POINT('Ctrl Pts',(-1.00129756308006,-0.308638795020976,
0.510906605094603));
#19356=CARTESIAN_POINT('Ctrl Pts',(-1.02374168767024,-0.308638795020976,
0.46430090015576));
#19357=CARTESIAN_POINT('Ctrl Pts',(-1.03504317708586,-0.305251990234488,
0.438600874831839));
#19358=CARTESIAN_POINT('Ctrl Pts',(-1.05494634094458,-0.290879136862659,
0.388295406390235));
#19359=CARTESIAN_POINT('Ctrl Pts',(-1.06356957703048,-0.279889827963178,
0.363699428370917));
#19360=CARTESIAN_POINT('Ctrl Pts',(-1.0788165083757,-0.251265615809407,
0.316022600643821));
#19361=CARTESIAN_POINT('Ctrl Pts',(-1.08664560412098,-0.227269801620063,
0.287406530683752));
#19362=CARTESIAN_POINT('Ctrl Pts',(-1.09728268713976,-0.177024326825049,
0.243890930799337));
#19363=CARTESIAN_POINT('Ctrl Pts',(-1.10139388218929,-0.144299303100741,
0.22376314604679));
#19364=CARTESIAN_POINT('Ctrl Pts',(-1.10509821673782,-0.0928409665394227,
0.204327142733961));
#19365=CARTESIAN_POINT('Ctrl Pts',(-1.10595102243643,-0.0762225747374254,
0.199591971170104));
#19366=CARTESIAN_POINT('Ctrl Pts',(-1.10653577764992,-0.0595300000000001,
0.196295654879792));
#19367=CARTESIAN_POINT('',(-1.123812,-0.05953,1.37627276864339E-16));
#19368=CARTESIAN_POINT('Origin',(0.,-0.05953,0.));
#19369=CARTESIAN_POINT('',(-1.123812,-0.35718,1.37627276864339E-16));
#19370=CARTESIAN_POINT('',(-1.123812,-0.208355,1.37627276864339E-16));
#19371=CARTESIAN_POINT('Origin',(0.,-0.35718,0.));
#19372=CARTESIAN_POINT('',(-1.10653577764992,-0.05953,-0.196295654879793));
#19373=CARTESIAN_POINT('Origin',(0.,-0.05953,0.));
#19374=CARTESIAN_POINT('',(-0.843383895613249,-0.05953,-0.742736168477219));
#19375=CARTESIAN_POINT('Ctrl Pts',(-1.10653577764992,-0.0595300000000001,
-0.196295654879792));
#19376=CARTESIAN_POINT('Ctrl Pts',(-1.10595102243643,-0.0762225747374255,
-0.199591971170104));
#19377=CARTESIAN_POINT('Ctrl Pts',(-1.10509821673782,-0.0928409665394228,
-0.204327142733962));
#19378=CARTESIAN_POINT('Ctrl Pts',(-1.10139388218929,-0.144299303100741,
-0.22376314604679));
#19379=CARTESIAN_POINT('Ctrl Pts',(-1.09728268713976,-0.177024326825049,
-0.243890930799338));
#19380=CARTESIAN_POINT('Ctrl Pts',(-1.08664560412098,-0.227269801620063,
-0.287406530683753));
#19381=CARTESIAN_POINT('Ctrl Pts',(-1.0788165083757,-0.251265615809407,
-0.316022600643821));
#19382=CARTESIAN_POINT('Ctrl Pts',(-1.06356957703048,-0.279889827963178,
-0.363699428370918));
#19383=CARTESIAN_POINT('Ctrl Pts',(-1.05494634094458,-0.290879136862659,
-0.388295406390235));
#19384=CARTESIAN_POINT('Ctrl Pts',(-1.03504317708586,-0.305251990234488,
-0.438600874831839));
#19385=CARTESIAN_POINT('Ctrl Pts',(-1.02374168767024,-0.308638795020976,
-0.46430090015576));
#19386=CARTESIAN_POINT('Ctrl Pts',(-1.00129756308006,-0.308638795020976,
-0.510906605094603));
#19387=CARTESIAN_POINT('Ctrl Pts',(-0.988250837578047,-0.305251990234488,
-0.535766169015486));
#19388=CARTESIAN_POINT('Ctrl Pts',(-0.961329858300736,-0.290879136862659,
-0.582692035672022));
#19389=CARTESIAN_POINT('Ctrl Pts',(-0.947476448101718,-0.279889827963178,
-0.604769294586516));
#19390=CARTESIAN_POINT('Ctrl Pts',(-0.919707509403859,-0.251265615809407,
-0.646415841396062));
#19391=CARTESIAN_POINT('Ctrl Pts',(-0.902215926359523,-0.227269801620064,
-0.670378702718353));
#19392=CARTESIAN_POINT('Ctrl Pts',(-0.87482617317514,-0.177024326825049,
-0.705826641853758));
#19393=CARTESIAN_POINT('Ctrl Pts',(-0.861652925570091,-0.144299303100741,
-0.721590372101268));
#19394=CARTESIAN_POINT('Ctrl Pts',(-0.848766861100456,-0.0928409665394229,
-0.736604687327351));
#19395=CARTESIAN_POINT('Ctrl Pts',(-0.84559647055299,-0.0762225747374255,
-0.740223768851063));
#19396=CARTESIAN_POINT('Ctrl Pts',(-0.843383895613249,-0.0595300000000001,
-0.742736168477219));
#19397=CARTESIAN_POINT('',(-0.536443649899847,-0.05953,-0.987512846410683));
#19398=CARTESIAN_POINT('Origin',(0.,-0.05953,0.));
#19399=CARTESIAN_POINT('',(0.0548532617164172,-0.05953,-1.12247250791415));
#19400=CARTESIAN_POINT('Ctrl Pts',(-0.536443649899848,-0.0595300000000001,
-0.987512846410683));
#19401=CARTESIAN_POINT('Ctrl Pts',(-0.533501897135712,-0.0762225747374254,
-0.989110885965947));
#19402=CARTESIAN_POINT('Ctrl Pts',(-0.529268075276156,-0.0928409665394227,
-0.991396466802469));
#19403=CARTESIAN_POINT('Ctrl Pts',(-0.511762781179147,-0.144299303100741,
-1.00061845128527));
#19404=CARTESIAN_POINT('Ctrl Pts',(-0.493462957200432,-0.177024326825049,
-1.0099536580922));
#19405=CARTESIAN_POINT('Ctrl Pts',(-0.45280897844858,-0.227269801620063,
-1.02876878445619));
#19406=CARTESIAN_POINT('Ctrl Pts',(-0.425554672694337,-0.251265615809407,
-1.04048957871266));
#19407=CARTESIAN_POINT('Ctrl Pts',(-0.3787731215897,-0.279889827963178,
-1.05829506364875));
#19408=CARTESIAN_POINT('Ctrl Pts',(-0.354166711873529,-0.290879136862659,
-1.06688848765783));
#19409=CARTESIAN_POINT('Ctrl Pts',(-0.302426893214944,-0.305251990234488,
-1.08269251410343));
#19410=CARTESIAN_POINT('Ctrl Pts',(-0.275287440920027,-0.308638795020976,
-1.0898803575765));
#19411=CARTESIAN_POINT('Ctrl Pts',(-0.224855950742601,-0.308638795020976,
-1.10139101611326));
#19412=CARTESIAN_POINT('Ctrl Pts',(-0.19728546073067,-0.305251990234488,
-1.10669035995599));
#19413=CARTESIAN_POINT('Ctrl Pts',(-0.143812384801039,-0.290879136862659,
-1.11490049012186));
#19414=CARTESIAN_POINT('Ctrl Pts',(-0.117914228755037,-0.279889827963178,
-1.1178344036749));
#19415=CARTESIAN_POINT('Ctrl Pts',(-0.0680399972366989,-0.251265615809407,
-1.12208997038458));
#19416=CARTESIAN_POINT('Ctrl Pts',(-0.0383992541984084,-0.227269801620063,
-1.12335509974011));
#19417=CARTESIAN_POINT('Ctrl Pts',(0.00639229239215326,-0.177024326825049,
-1.12404235695137));
#19418=CARTESIAN_POINT('Ctrl Pts',(0.0269302585198977,-0.144299303100741,
-1.12357162229597));
#19419=CARTESIAN_POINT('Ctrl Pts',(0.04670325263426,-0.0928409665394228,
-1.12285816383385));
#19420=CARTESIAN_POINT('Ctrl Pts',(0.0515094706813703,-0.0762225747374255,
-1.12263591311425));
#19421=CARTESIAN_POINT('Ctrl Pts',(0.0548532617164176,-0.0595300000000001,
-1.12247250791414));
#19422=CARTESIAN_POINT('',(0.437601487681057,-0.05953,-1.03511272300331));
#19423=CARTESIAN_POINT('Origin',(0.,-0.05953,0.));
#19424=CARTESIAN_POINT('',(0.911784794170997,-0.05953,-0.656964154625313));
#19425=CARTESIAN_POINT('Ctrl Pts',(0.437601487681056,-0.0595300000000001,
-1.03511272300331));
#19426=CARTESIAN_POINT('Ctrl Pts',(0.440685038163619,-0.0762225747374255,
-1.03380912944435));
#19427=CARTESIAN_POINT('Ctrl Pts',(0.445111721969657,-0.0928409665394228,
-1.03192403056628));
#19428=CARTESIAN_POINT('Ctrl Pts',(0.463236132117164,-0.144299303100741,
-1.0239876538093));
#19429=CARTESIAN_POINT('Ctrl Pts',(0.481944444320713,-0.177024326825049,
-1.01550068154148));
#19430=CARTESIAN_POINT('Ctrl Pts',(0.522002043615455,-0.227269801620064,
-0.995447160474328));
#19431=CARTESIAN_POINT('Ctrl Pts',(0.548158511259203,-0.251265615809407,
-0.981446681891443));
#19432=CARTESIAN_POINT('Ctrl Pts',(0.591247219971725,-0.279889827963178,
-0.955972930713954));
#19433=CARTESIAN_POINT('Ctrl Pts',(0.613307674922609,-0.290879136862659,
-0.942092777160053));
#19434=CARTESIAN_POINT('Ctrl Pts',(0.657923009631182,-0.305251990234487,
-0.91149460735272));
#19435=CARTESIAN_POINT('Ctrl Pts',(0.680463863683393,-0.308638795020976,
-0.894757676234429));
#19436=CARTESIAN_POINT('Ctrl Pts',(0.720906778729542,-0.308638795020976,
-0.862505527716294));
#19437=CARTESIAN_POINT('Ctrl Pts',(0.742239891936899,-0.305251990234488,
-0.844254137480381));
#19438=CARTESIAN_POINT('Ctrl Pts',(0.781998747691872,-0.290879136862659,
-0.80756613568454));
#19439=CARTESIAN_POINT('Ctrl Pts',(0.800439809856112,-0.279889827963178,
-0.789147407129765));
#19440=CARTESIAN_POINT('Ctrl Pts',(0.834863020612702,-0.251265615809407,
-0.752807465209441));
#19441=CARTESIAN_POINT('Ctrl Pts',(0.854332839576145,-0.227269801620064,
-0.73042219438957));
#19442=CARTESIAN_POINT('Ctrl Pts',(0.882797231409153,-0.177024326825049,
-0.695831250979106));
#19443=CARTESIAN_POINT('Ctrl Pts',(0.895234408667242,-0.144299303100741,
-0.679480524217551));
#19444=CARTESIAN_POINT('Ctrl Pts',(0.907004864562642,-0.0928409665394228,
-0.663576540841106));
#19445=CARTESIAN_POINT('Ctrl Pts',(0.909827729890942,-0.0762225747374256,
-0.659680317203144));
#19446=CARTESIAN_POINT('Ctrl Pts',(0.911784794170998,-0.0595300000000001,
-0.656964154625312));
#19447=CARTESIAN_POINT('',(1.08212377959455,-0.05953,-0.303251606722892));
#19448=CARTESIAN_POINT('Origin',(0.,-0.05953,0.));
#19449=CARTESIAN_POINT('',(1.08212377959455,-0.05953,0.303251606722892));
#19450=CARTESIAN_POINT('Ctrl Pts',(1.08212377959455,-0.0595300000000001,
-0.303251606722892));
#19451=CARTESIAN_POINT('Ctrl Pts',(1.0830271513892,-0.0762225747374255,
-0.300028012588062));
#19452=CARTESIAN_POINT('Ctrl Pts',(1.08431331394788,-0.0928409665394228,
-0.2953917518996));
#19453=CARTESIAN_POINT('Ctrl Pts',(1.08940878963422,-0.144299303100741,
-0.276273267473431));
#19454=CARTESIAN_POINT('Ctrl Pts',(1.09443784939331,-0.177024326825049,
-0.256354979351213));
#19455=CARTESIAN_POINT('Ctrl Pts',(1.10373487993589,-0.227269801620064,
-0.212533521233765));
#19456=CARTESIAN_POINT('Ctrl Pts',(1.10909715583869,-0.251265615809407,
-0.183354415742157));
#19457=CARTESIAN_POINT('Ctrl Pts',(1.1160463456491,-0.279889827963178,-0.133783682657561));
#19458=CARTESIAN_POINT('Ctrl Pts',(1.11894887330541,-0.290879136862659,
-0.107881990270302));
#19459=CARTESIAN_POINT('Ctrl Pts',(1.12284346704144,-0.305251990234488,
-0.0539226701638766));
#19460=CARTESIAN_POINT('Ctrl Pts',(1.123812,-0.308638795020976,-0.025864214957475));
#19461=CARTESIAN_POINT('Ctrl Pts',(1.123812,-0.308638795020976,0.025864214957475));
#19462=CARTESIAN_POINT('Ctrl Pts',(1.12284346704144,-0.305251990234488,
0.0539226701638766));
#19463=CARTESIAN_POINT('Ctrl Pts',(1.11894887330541,-0.290879136862659,
0.107881990270302));
#19464=CARTESIAN_POINT('Ctrl Pts',(1.1160463456491,-0.279889827963178,0.133783682657561));
#19465=CARTESIAN_POINT('Ctrl Pts',(1.10909715583869,-0.251265615809407,
0.183354415742157));
#19466=CARTESIAN_POINT('Ctrl Pts',(1.10373487993589,-0.227269801620064,
0.212533521233765));
#19467=CARTESIAN_POINT('Ctrl Pts',(1.09443784939331,-0.177024326825049,
0.256354979351213));
#19468=CARTESIAN_POINT('Ctrl Pts',(1.08940878963422,-0.144299303100741,
0.276273267473431));
#19469=CARTESIAN_POINT('Ctrl Pts',(1.08431331394788,-0.0928409665394228,
0.2953917518996));
#19470=CARTESIAN_POINT('Ctrl Pts',(1.0830271513892,-0.0762225747374255,
0.300028012588062));
#19471=CARTESIAN_POINT('Ctrl Pts',(1.08212377959455,-0.0595300000000001,
0.303251606722892));
#19472=CARTESIAN_POINT('Origin',(0.,-0.05953,0.));
#19473=CARTESIAN_POINT('Origin',(0.,-0.05953,0.));
#19474=CARTESIAN_POINT('',(0.0589974094846122,-0.05953,1.07456964270265));
#19475=CARTESIAN_POINT('Origin',(0.,-0.05953,0.));
#19476=CARTESIAN_POINT('Origin',(-0.244773027351946,-0.05953,1.07242070340001));
#19477=CARTESIAN_POINT('Origin',(-0.244773027351946,0.,1.07242070340001));
#19478=CARTESIAN_POINT('',(-0.519393123750572,-0.05953,0.942555777842682));
#19479=CARTESIAN_POINT('Ctrl Pts',(-0.519393123750572,-0.05953,0.942555777842682));
#19480=CARTESIAN_POINT('Ctrl Pts',(-0.513714466572041,-0.0925528133349865,
0.945684988399766));
#19481=CARTESIAN_POINT('Ctrl Pts',(-0.503136848051455,-0.124911173756694,
0.951483858396181));
#19482=CARTESIAN_POINT('Ctrl Pts',(-0.47593627990192,-0.177924977804098,
0.965323333309091));
#19483=CARTESIAN_POINT('Ctrl Pts',(-0.460931856495794,-0.199697230012983,
0.972669835243841));
#19484=CARTESIAN_POINT('Ctrl Pts',(-0.426157505475872,-0.237895043532788,
0.988400002689705));
#19485=CARTESIAN_POINT('Ctrl Pts',(-0.406380688682952,-0.254319232363049,
0.996771768218699));
#19486=CARTESIAN_POINT('Ctrl Pts',(-0.364750145543744,-0.28018331644634,
1.01272583306292));
#19487=CARTESIAN_POINT('Ctrl Pts',(-0.340838910881557,-0.29104845371857,
1.02112815447116));
#19488=CARTESIAN_POINT('Ctrl Pts',(-0.290495481564827,-0.30527573347708,
1.036574285215));
#19489=CARTESIAN_POINT('Ctrl Pts',(-0.264056468041074,-0.308638795020976,
1.04359501395068));
#19490=CARTESIAN_POINT('Ctrl Pts',(-0.214892249704082,-0.308638795020976,
1.05481642595959));
#19491=CARTESIAN_POINT('Ctrl Pts',(-0.188025341585962,-0.30527573347708,
1.05996242598502));
#19492=CARTESIAN_POINT('Ctrl Pts',(-0.135965654106109,-0.29104845371857,
1.06788913840721));
#19493=CARTESIAN_POINT('Ctrl Pts',(-0.110776745452494,-0.28018331644634,
1.07069360430242));
#19494=CARTESIAN_POINT('Ctrl Pts',(-0.0663467128214646,-0.254319232363049,
1.07438230428002));
#19495=CARTESIAN_POINT('Ctrl Pts',(-0.0448960436540983,-0.237895043532788,
1.07542044338697));
#19496=CARTESIAN_POINT('Ctrl Pts',(-0.00674037211528124,-0.199697230012983,
1.07633607767727));
#19497=CARTESIAN_POINT('Ctrl Pts',(0.00996567398334777,-0.177924977804098,
1.07622728347683));
#19498=CARTESIAN_POINT('Ctrl Pts',(0.0404772621979741,-0.124911173756694,
1.07556023164702));
#19499=CARTESIAN_POINT('Ctrl Pts',(0.0525234025782719,-0.0925528133349865,
1.07492508698591));
#19500=CARTESIAN_POINT('Ctrl Pts',(0.0589974094846124,-0.05953,1.07456964270265));
#19501=CARTESIAN_POINT('Origin',(-0.244773027351946,-0.05953,1.07242070340001));
#19502=CARTESIAN_POINT('Origin',(0.,-0.05953,0.));
#19503=CARTESIAN_POINT('',(-0.803348093619616,-0.05953,0.716109245731214));
#19504=CARTESIAN_POINT('Origin',(0.,-0.05953,0.));
#19505=CARTESIAN_POINT('Origin',(-0.991065754692661,-0.05953,0.477272113029314));
#19506=CARTESIAN_POINT('Origin',(-0.991065754692661,0.,0.477272113029314));
#19507=CARTESIAN_POINT('',(-1.06075609691358,-0.05953,0.181596019242328));
#19508=CARTESIAN_POINT('Ctrl Pts',(-1.06075609691358,-0.05953,0.181596019242328));
#19509=CARTESIAN_POINT('Ctrl Pts',(-1.05966202740332,-0.0925528133349865,
0.187986803072856));
#19510=CARTESIAN_POINT('Ctrl Pts',(-1.05760072925372,-0.124911173756694,
0.199872254546857));
#19511=CARTESIAN_POINT('Ctrl Pts',(-1.05146158959546,-0.177924977804098,
0.22976728653846));
#19512=CARTESIAN_POINT('Ctrl Pts',(-1.04785021111757,-0.199697230012983,
0.246078686169301));
#19513=CARTESIAN_POINT('Ctrl Pts',(-1.03846709802406,-0.237895043532788,
0.283073967563097));
#19514=CARTESIAN_POINT('Ctrl Pts',(-1.03268176429485,-0.254319232363049,
0.303755815985685));
#19515=CARTESIAN_POINT('Ctrl Pts',(-1.01919893537026,-0.28018331644634,
0.346251081972725));
#19516=CARTESIAN_POINT('Ctrl Pts',(-1.01085972381132,-0.29104845371857,
0.370184399726282));
#19517=CARTESIAN_POINT('Ctrl Pts',(-0.99154738033959,-0.30527573347708,
0.419174982698463));
#19518=CARTESIAN_POINT('Ctrl Pts',(-0.980551951791748,-0.308638795020976,
0.444223188605045));
#19519=CARTESIAN_POINT('Ctrl Pts',(-0.958671816228589,-0.308638795020976,
0.489657758261848));
#19520=CARTESIAN_POINT('Ctrl Pts',(-0.945943877838127,-0.30527573347708,
0.51387163140139));
#19521=CARTESIAN_POINT('Ctrl Pts',(-0.91968254693063,-0.29104845371857,
0.559515758398093));
#19522=CARTESIAN_POINT('Ctrl Pts',(-0.906170138993533,-0.28018331644634,
0.580957796077825));
#19523=CARTESIAN_POINT('Ctrl Pts',(-0.8813524085237,-0.254319232363049,
0.617994461173994));
#19524=CARTESIAN_POINT('Ctrl Pts',(-0.868789784891799,-0.237895043532788,
0.635412538795143));
#19525=CARTESIAN_POINT('Ctrl Pts',(-0.845715984518854,-0.199697230012983,
0.66581473268113));
#19526=CARTESIAN_POINT('Ctrl Pts',(-0.835214876415962,-0.177924977804098,
0.678808213394124));
#19527=CARTESIAN_POINT('Ctrl Pts',(-0.815669690204649,-0.124911173756694,
0.702247233627224));
#19528=CARTESIAN_POINT('Ctrl Pts',(-0.807662468433796,-0.0925528133349865,
0.711269279199861));
#19529=CARTESIAN_POINT('Ctrl Pts',(-0.803348093619616,-0.05953,0.716109245731214));
#19530=CARTESIAN_POINT('Origin',(-0.991065754692661,-0.05953,0.477272113029314));
#19531=CARTESIAN_POINT('Origin',(0.,-0.05953,0.));
#19532=CARTESIAN_POINT('',(-1.076188,-0.05953,1.31795018948079E-16));
#19533=CARTESIAN_POINT('Origin',(0.,-0.05953,0.));
#19534=CARTESIAN_POINT('',(-1.06075609691358,-0.05953,-0.181596019242328));
#19535=CARTESIAN_POINT('Origin',(0.,-0.05953,0.));
#19536=CARTESIAN_POINT('Origin',(-0.991065754692661,-0.05953,-0.477272113029314));
#19537=CARTESIAN_POINT('Origin',(-0.991065754692661,0.,-0.477272113029314));
#19538=CARTESIAN_POINT('',(-0.803348093619616,-0.05953,-0.716109245731215));
#19539=CARTESIAN_POINT('Ctrl Pts',(-0.803348093619616,-0.05953,-0.716109245731215));
#19540=CARTESIAN_POINT('Ctrl Pts',(-0.807662468433795,-0.0925528133349865,
-0.711269279199862));
#19541=CARTESIAN_POINT('Ctrl Pts',(-0.815669690204649,-0.124911173756694,
-0.702247233627224));
#19542=CARTESIAN_POINT('Ctrl Pts',(-0.835214876415962,-0.177924977804098,
-0.678808213394124));
#19543=CARTESIAN_POINT('Ctrl Pts',(-0.845715984518854,-0.199697230012983,
-0.66581473268113));
#19544=CARTESIAN_POINT('Ctrl Pts',(-0.868789784891799,-0.237895043532788,
-0.635412538795143));
#19545=CARTESIAN_POINT('Ctrl Pts',(-0.8813524085237,-0.254319232363049,
-0.617994461173994));
#19546=CARTESIAN_POINT('Ctrl Pts',(-0.906170138993533,-0.28018331644634,
-0.580957796077826));
#19547=CARTESIAN_POINT('Ctrl Pts',(-0.91968254693063,-0.29104845371857,
-0.559515758398093));
#19548=CARTESIAN_POINT('Ctrl Pts',(-0.945943877838127,-0.30527573347708,
-0.51387163140139));
#19549=CARTESIAN_POINT('Ctrl Pts',(-0.958671816228589,-0.308638795020976,
-0.489657758261848));
#19550=CARTESIAN_POINT('Ctrl Pts',(-0.980551951791748,-0.308638795020976,
-0.444223188605045));
#19551=CARTESIAN_POINT('Ctrl Pts',(-0.99154738033959,-0.30527573347708,
-0.419174982698463));
#19552=CARTESIAN_POINT('Ctrl Pts',(-1.01085972381132,-0.29104845371857,
-0.370184399726282));
#19553=CARTESIAN_POINT('Ctrl Pts',(-1.01919893537026,-0.28018331644634,
-0.346251081972725));
#19554=CARTESIAN_POINT('Ctrl Pts',(-1.03268176429485,-0.254319232363049,
-0.303755815985685));
#19555=CARTESIAN_POINT('Ctrl Pts',(-1.03846709802406,-0.237895043532788,
-0.283073967563097));
#19556=CARTESIAN_POINT('Ctrl Pts',(-1.04785021111757,-0.199697230012983,
-0.246078686169302));
#19557=CARTESIAN_POINT('Ctrl Pts',(-1.05146158959546,-0.177924977804098,
-0.229767286538461));
#19558=CARTESIAN_POINT('Ctrl Pts',(-1.05760072925372,-0.124911173756694,
-0.199872254546858));
#19559=CARTESIAN_POINT('Ctrl Pts',(-1.05966202740332,-0.0925528133349864,
-0.187986803072857));
#19560=CARTESIAN_POINT('Ctrl Pts',(-1.06075609691358,-0.05953,-0.181596019242328));
#19561=CARTESIAN_POINT('Origin',(-0.991065754692661,-0.05953,-0.477272113029314));
#19562=CARTESIAN_POINT('Origin',(0.,-0.05953,0.));
#19563=CARTESIAN_POINT('',(-0.519393123750572,-0.05953,-0.942555777842682));
#19564=CARTESIAN_POINT('Origin',(0.,-0.05953,0.));
#19565=CARTESIAN_POINT('Origin',(-0.244773027351946,-0.05953,-1.07242070340001));
#19566=CARTESIAN_POINT('Origin',(-0.244773027351946,0.,-1.07242070340001));
#19567=CARTESIAN_POINT('',(0.0589974094846125,-0.05953,-1.07456964270265));
#19568=CARTESIAN_POINT('Ctrl Pts',(0.0589974094846127,-0.05953,-1.07456964270265));
#19569=CARTESIAN_POINT('Ctrl Pts',(0.0525234025782722,-0.0925528133349865,
-1.07492508698591));
#19570=CARTESIAN_POINT('Ctrl Pts',(0.0404772621979744,-0.124911173756694,
-1.07556023164702));
#19571=CARTESIAN_POINT('Ctrl Pts',(0.0099656739833481,-0.177924977804098,
-1.07622728347683));
#19572=CARTESIAN_POINT('Ctrl Pts',(-0.00674037211528096,-0.199697230012983,
-1.07633607767727));
#19573=CARTESIAN_POINT('Ctrl Pts',(-0.044896043654098,-0.237895043532788,
-1.07542044338697));
#19574=CARTESIAN_POINT('Ctrl Pts',(-0.0663467128214644,-0.254319232363049,
-1.07438230428002));
#19575=CARTESIAN_POINT('Ctrl Pts',(-0.110776745452493,-0.28018331644634,
-1.07069360430242));
#19576=CARTESIAN_POINT('Ctrl Pts',(-0.135965654106109,-0.29104845371857,
-1.06788913840721));
#19577=CARTESIAN_POINT('Ctrl Pts',(-0.188025341585962,-0.30527573347708,
-1.05996242598502));
#19578=CARTESIAN_POINT('Ctrl Pts',(-0.214892249704082,-0.308638795020976,
-1.05481642595959));
#19579=CARTESIAN_POINT('Ctrl Pts',(-0.264056468041074,-0.308638795020976,
-1.04359501395068));
#19580=CARTESIAN_POINT('Ctrl Pts',(-0.290495481564827,-0.30527573347708,
-1.036574285215));
#19581=CARTESIAN_POINT('Ctrl Pts',(-0.340838910881557,-0.291048453718569,
-1.02112815447116));
#19582=CARTESIAN_POINT('Ctrl Pts',(-0.364750145543744,-0.28018331644634,
-1.01272583306292));
#19583=CARTESIAN_POINT('Ctrl Pts',(-0.406380688682952,-0.254319232363049,
-0.996771768218699));
#19584=CARTESIAN_POINT('Ctrl Pts',(-0.426157505475872,-0.237895043532788,
-0.988400002689705));
#19585=CARTESIAN_POINT('Ctrl Pts',(-0.460931856495794,-0.199697230012983,
-0.972669835243841));
#19586=CARTESIAN_POINT('Ctrl Pts',(-0.475936279901919,-0.177924977804098,
-0.965323333309091));
#19587=CARTESIAN_POINT('Ctrl Pts',(-0.503136848051454,-0.124911173756694,
-0.951483858396181));
#19588=CARTESIAN_POINT('Ctrl Pts',(-0.513714466572041,-0.0925528133349865,
-0.945684988399766));
#19589=CARTESIAN_POINT('Ctrl Pts',(-0.519393123750572,-0.05953,-0.942555777842682));
#19590=CARTESIAN_POINT('Origin',(-0.244773027351946,-0.05953,-1.07242070340001));
#19591=CARTESIAN_POINT('Origin',(0.,-0.05953,0.));
#19592=CARTESIAN_POINT('',(0.413083465285518,-0.05953,-0.993751811093549));
#19593=CARTESIAN_POINT('Origin',(0.,-0.05953,0.));
#19594=CARTESIAN_POINT('Origin',(0.685838782044607,-0.05953,-0.860014630714833));
#19595=CARTESIAN_POINT('Origin',(0.685838782044607,0.,-0.860014630714833));
#19596=CARTESIAN_POINT('',(0.876916659919095,-0.05953,-0.623857181492959));
#19597=CARTESIAN_POINT('Ctrl Pts',(0.876916659919095,-0.05953,-0.623857181492958));
#19598=CARTESIAN_POINT('Ctrl Pts',(0.873158080166742,-0.0925528133349865,
-0.62914037979579));
#19599=CARTESIAN_POINT('Ctrl Pts',(0.866144010579847,-0.124911173756694,
-0.638954437806245));
#19600=CARTESIAN_POINT('Ctrl Pts',(0.847641868610495,-0.177924977804098,
-0.663225258065736));
#19601=CARTESIAN_POINT('Ctrl Pts',(0.837310877969633,-0.199697230012983,
-0.676354402927683));
#19602=CARTESIAN_POINT('Ctrl Pts',(0.81280533416753,-0.237895043532788,
-0.705614819529209));
#19603=CARTESIAN_POINT('Ctrl Pts',(0.798619410861634,-0.254319232363049,
-0.721738358858166));
#19604=CARTESIAN_POINT('Ctrl Pts',(0.768033796848072,-0.28018331644634,
-0.754175290318038));
#19605=CARTESIAN_POINT('Ctrl Pts',(0.750136149454208,-0.29104845371857,
-0.772120216227122));
#19606=CARTESIAN_POINT('Ctrl Pts',(0.711480111898423,-0.30527573347708,
-0.807879894508811));
#19607=CARTESIAN_POINT('Ctrl Pts',(0.690705563850638,-0.308638795020976,
-0.825676810575913));
#19608=CARTESIAN_POINT('Ctrl Pts',(0.651278921914856,-0.308638795020976,
-0.857118508332695));
#19609=CARTESIAN_POINT('Ctrl Pts',(0.629305439856167,-0.30527573347708,
-0.873412008702649));
#19610=CARTESIAN_POINT('Ctrl Pts',(0.585840553788742,-0.29104845371857,
-0.903141581680914));
#19611=CARTESIAN_POINT('Ctrl Pts',(0.564362943424239,-0.28018331644634,
-0.916597376014514));
#19612=CARTESIAN_POINT('Ctrl Pts',(0.525933334162556,-0.254319232363049,
-0.939198248544427));
#19613=CARTESIAN_POINT('Ctrl Pts',(0.507057380724533,-0.237895043532788,
-0.949440676105255));
#19614=CARTESIAN_POINT('Ctrl Pts',(0.473077587363686,-0.199697230012983,
-0.966820759530997));
#19615=CARTESIAN_POINT('Ctrl Pts',(0.457978755888596,-0.177924977804098,
-0.973971221090534));
#19616=CARTESIAN_POINT('Ctrl Pts',(0.430199341854858,-0.124911173756694,
-0.986608710139579));
#19617=CARTESIAN_POINT('Ctrl Pts',(0.419070565453384,-0.0925528133349865,
-0.991263089003441));
#19618=CARTESIAN_POINT('Ctrl Pts',(0.413083465285518,-0.05953,-0.993751811093549));
#19619=CARTESIAN_POINT('Origin',(0.685838782044607,-0.05953,-0.860014630714833));
#19620=CARTESIAN_POINT('Origin',(0.,-0.208355,0.));
#19621=CARTESIAN_POINT('',(-1.076188,-0.35718,1.31795018948079E-16));
#19622=CARTESIAN_POINT('Origin',(0.,-0.35718,0.));
#19623=CARTESIAN_POINT('',(-1.076188,-0.208355,1.31795018948079E-16));
#19624=CARTESIAN_POINT('',(1.03449977959455,-0.05953,0.296632461748266));
#19625=CARTESIAN_POINT('Origin',(0.,-0.05953,0.));
#19626=CARTESIAN_POINT('',(1.03449977959455,-0.05953,-0.296632461748266));
#19627=CARTESIAN_POINT('Ctrl Pts',(1.03449977959455,-0.05953,0.296632461748267));
#19628=CARTESIAN_POINT('Ctrl Pts',(1.03628691421076,-0.0925528133349865,
0.290399865505497));
#19629=CARTESIAN_POINT('Ctrl Pts',(1.03958665287714,-0.124911173756694,
0.278797079997872));
#19630=CARTESIAN_POINT('Ctrl Pts',(1.0470264474309,-0.177924977804098,0.249198913998601));
#19631=CARTESIAN_POINT('Ctrl Pts',(1.05084995891418,-0.199697230012983,
0.232935932341942));
#19632=CARTESIAN_POINT('Ctrl Pts',(1.05844771715377,-0.237895043532788,
0.195533155353269));
#19633=CARTESIAN_POINT('Ctrl Pts',(1.06220882929878,-0.254319232363049,
0.17438929156337));
#19634=CARTESIAN_POINT('Ctrl Pts',(1.06849922508772,-0.28018331644634,0.130252399648131));
#19635=CARTESIAN_POINT('Ctrl Pts',(1.07137013248666,-0.29104845371857,0.105070977154072));
#19636=CARTESIAN_POINT('Ctrl Pts',(1.07522652957392,-0.30527573347708,0.0525526752791107));
#19637=CARTESIAN_POINT('Ctrl Pts',(1.076188,-0.308638795020976,0.025214283908933));
#19638=CARTESIAN_POINT('Ctrl Pts',(1.076188,-0.308638795020976,-0.025214283908933));
#19639=CARTESIAN_POINT('Ctrl Pts',(1.07522652957392,-0.30527573347708,-0.0525526752791107));
#19640=CARTESIAN_POINT('Ctrl Pts',(1.07137013248666,-0.29104845371857,-0.105070977154072));
#19641=CARTESIAN_POINT('Ctrl Pts',(1.06849922508772,-0.28018331644634,-0.130252399648131));
#19642=CARTESIAN_POINT('Ctrl Pts',(1.06220882929878,-0.254319232363049,
-0.17438929156337));
#19643=CARTESIAN_POINT('Ctrl Pts',(1.05844771715377,-0.237895043532788,
-0.195533155353269));
#19644=CARTESIAN_POINT('Ctrl Pts',(1.05084995891418,-0.199697230012983,
-0.232935932341942));
#19645=CARTESIAN_POINT('Ctrl Pts',(1.0470264474309,-0.177924977804098,-0.249198913998601));
#19646=CARTESIAN_POINT('Ctrl Pts',(1.03958665287714,-0.124911173756694,
-0.278797079997872));
#19647=CARTESIAN_POINT('Ctrl Pts',(1.03628691421076,-0.0925528133349865,
-0.290399865505497));
#19648=CARTESIAN_POINT('Ctrl Pts',(1.03449977959455,-0.05953,-0.296632461748267));
#19649=CARTESIAN_POINT('Origin',(0.,-0.05953,0.));
#19650=CARTESIAN_POINT('Origin',(0.,-0.05953,0.));
#19651=CARTESIAN_POINT('Origin',(1.1,-0.05953,0.));
#19652=CARTESIAN_POINT('Origin',(1.1,0.,0.));
#19653=CARTESIAN_POINT('Origin',(1.1,-0.05953,0.));
#19654=CARTESIAN_POINT('Origin',(0.,-0.35718,0.));
#19655=CARTESIAN_POINT('Origin',(0.,-0.05953,0.));
#19656=CARTESIAN_POINT('',(0.,0.,0.));
#19657=CARTESIAN_POINT('Origin',(1.119765,0.495,0.));
#19658=CARTESIAN_POINT('',(-1.119765,0.495,-1.37131662304724E-16));
#19659=CARTESIAN_POINT('Origin',(0.,0.495,0.));
#19660=CARTESIAN_POINT('',(-1.085235,0.495,-1.32902956907268E-16));
#19661=CARTESIAN_POINT('Origin',(0.,0.495,0.));
#19662=CARTESIAN_POINT('Origin',(0.,0.4575,0.));
#19663=CARTESIAN_POINT('',(-1.119765,0.42,-1.37131662304724E-16));
#19664=CARTESIAN_POINT('Origin',(0.,0.42,0.));
#19665=CARTESIAN_POINT('',(-1.119765,0.4575,-1.37131662304724E-16));
#19666=CARTESIAN_POINT('Origin',(1.085235,0.42,0.));
#19667=CARTESIAN_POINT('',(-1.085235,0.42,-1.32902956907268E-16));
#19668=CARTESIAN_POINT('Origin',(0.,0.42,0.));
#19669=CARTESIAN_POINT('Origin',(0.,0.4575,0.));
#19670=CARTESIAN_POINT('',(-1.085235,0.4575,-1.32902956907268E-16));
#19671=CARTESIAN_POINT('Origin',(1.119765,-0.42,0.));
#19672=CARTESIAN_POINT('',(-1.119765,-0.42,-1.37131662304724E-16));
#19673=CARTESIAN_POINT('Origin',(0.,-0.42,0.));
#19674=CARTESIAN_POINT('',(-1.085235,-0.42,-1.32902956907268E-16));
#19675=CARTESIAN_POINT('Origin',(0.,-0.42,0.));
#19676=CARTESIAN_POINT('Origin',(0.,-0.4575,0.));
#19677=CARTESIAN_POINT('',(-1.119765,-0.495,-1.37131662304724E-16));
#19678=CARTESIAN_POINT('Origin',(0.,-0.495,0.));
#19679=CARTESIAN_POINT('',(-1.119765,-0.4575,-1.37131662304724E-16));
#19680=CARTESIAN_POINT('Origin',(1.085235,-0.495,0.));
#19681=CARTESIAN_POINT('',(-1.085235,-0.495,-1.32902956907268E-16));
#19682=CARTESIAN_POINT('Origin',(0.,-0.495,0.));
#19683=CARTESIAN_POINT('Origin',(0.,-0.4575,0.));
#19684=CARTESIAN_POINT('',(-1.085235,-0.4575,-1.32902956907268E-16));
#19685=CARTESIAN_POINT('',(0.,0.,0.));
#19686=CARTESIAN_POINT('',(0.,0.,0.));
#19687=CARTESIAN_POINT('',(0.,0.,0.));
#19688=CARTESIAN_POINT('',(0.,0.,0.));
#19689=CARTESIAN_POINT('',(0.,0.,0.));
#19690=CARTESIAN_POINT('',(0.,0.,0.));
#19691=CARTESIAN_POINT('Origin',(0.0866025403784439,-0.4,-0.15));
#19692=CARTESIAN_POINT('',(0.173205080756888,-0.4,0.));
#19693=CARTESIAN_POINT('',(0.0866025403784439,-0.4,-0.15));
#19694=CARTESIAN_POINT('',(0.173205080756888,-0.4,0.));
#19695=CARTESIAN_POINT('',(0.0866025403784439,-0.64,-0.15));
#19696=CARTESIAN_POINT('',(0.0866025403784439,-0.4,-0.15));
#19697=CARTESIAN_POINT('',(0.173205080756888,-0.64,0.));
#19698=CARTESIAN_POINT('',(0.173205080756888,-0.64,0.));
#19699=CARTESIAN_POINT('',(0.173205080756888,-0.4,0.));
#19700=CARTESIAN_POINT('Origin',(-0.0866025403784438,-0.4,-0.15));
#19701=CARTESIAN_POINT('',(-0.0866025403784438,-0.4,-0.15));
#19702=CARTESIAN_POINT('',(0.0866025403784439,-0.4,-0.15));
#19703=CARTESIAN_POINT('',(-0.0866025403784438,-0.64,-0.15));
#19704=CARTESIAN_POINT('',(-0.0866025403784438,-0.4,-0.15));
#19705=CARTESIAN_POINT('',(0.0866025403784439,-0.64,-0.15));
#19706=CARTESIAN_POINT('Origin',(-0.173205080756888,-0.4,-2.77555756156289E-17));
#19707=CARTESIAN_POINT('',(-0.173205080756888,-0.4,-2.12115047744981E-17));
#19708=CARTESIAN_POINT('',(-0.0866025403784438,-0.4,-0.15));
#19709=CARTESIAN_POINT('',(-0.173205080756888,-0.64,-2.77555756156289E-17));
#19710=CARTESIAN_POINT('',(-0.173205080756888,-0.4,-2.12115047744981E-17));
#19711=CARTESIAN_POINT('',(-0.0866025403784438,-0.64,-0.15));
#19712=CARTESIAN_POINT('Origin',(-0.0866025403784439,-0.4,0.15));
#19713=CARTESIAN_POINT('',(-0.0866025403784439,-0.4,0.15));
#19714=CARTESIAN_POINT('',(-0.173205080756888,-0.4,-2.12115047744981E-17));
#19715=CARTESIAN_POINT('',(-0.0866025403784439,-0.64,0.15));
#19716=CARTESIAN_POINT('',(-0.0866025403784439,-0.4,0.15));
#19717=CARTESIAN_POINT('',(-0.173205080756888,-0.64,-2.12115047744981E-17));
#19718=CARTESIAN_POINT('Origin',(0.0866025403784439,-0.4,0.15));
#19719=CARTESIAN_POINT('',(0.0866025403784439,-0.4,0.15));
#19720=CARTESIAN_POINT('',(-0.0866025403784439,-0.4,0.15));
#19721=CARTESIAN_POINT('',(0.0866025403784439,-0.64,0.15));
#19722=CARTESIAN_POINT('',(0.0866025403784439,-0.4,0.15));
#19723=CARTESIAN_POINT('',(-0.0866025403784439,-0.64,0.15));
#19724=CARTESIAN_POINT('Origin',(0.173205080756888,-0.4,0.));
#19725=CARTESIAN_POINT('',(0.0866025403784439,-0.4,0.15));
#19726=CARTESIAN_POINT('',(0.0866025403784439,-0.64,0.15));
#19727=CARTESIAN_POINT('Origin',(0.,-0.4,-2.77555756156289E-17));
#19728=CARTESIAN_POINT('Origin',(0.,-0.64,-2.77555756156289E-17));
#19729=CARTESIAN_POINT('Origin',(0.,-1.,0.));
#19730=CARTESIAN_POINT('',(-0.1954,-1.,2.39295984553393E-17));
#19731=CARTESIAN_POINT('Origin',(0.,-1.,0.));
#19732=CARTESIAN_POINT('Origin',(0.3,0.4,0.));
#19733=CARTESIAN_POINT('',(-0.3,0.4,-3.67394039744206E-17));
#19734=CARTESIAN_POINT('Origin',(0.,0.4,0.));
#19735=CARTESIAN_POINT('Origin',(0.,0.375,0.));
#19736=CARTESIAN_POINT('',(-0.35,0.35,-4.28626379701573E-17));
#19737=CARTESIAN_POINT('Origin',(0.,0.35,0.));
#19738=CARTESIAN_POINT('',(-0.325,0.375,-3.9801020972289E-17));
#19739=CARTESIAN_POINT('Origin',(0.,0.19,0.));
#19740=CARTESIAN_POINT('',(-0.35,0.03,-4.28626379701574E-17));
#19741=CARTESIAN_POINT('Origin',(0.,0.03,0.));
#19742=CARTESIAN_POINT('',(-0.35,0.19,-4.28626379701574E-17));
#19743=CARTESIAN_POINT('Origin',(0.,0.0149999999999999,0.));
#19744=CARTESIAN_POINT('',(-0.32,-3.29597460435593E-17,-3.91886975727153E-17));
#19745=CARTESIAN_POINT('Origin',(0.,0.,0.));
#19746=CARTESIAN_POINT('',(-0.335,0.0149999999999999,-4.10256677714363E-17));
#19747=CARTESIAN_POINT('Origin',(0.22,0.,0.));
#19748=CARTESIAN_POINT('',(-0.22,-6.93889390390723E-18,-2.69422295812418E-17));
#19749=CARTESIAN_POINT('Origin',(0.,0.,0.));
#19750=CARTESIAN_POINT('Origin',(0.,-0.02,0.));
#19751=CARTESIAN_POINT('',(-0.1954,-0.0492,2.39295984553393E-17));
#19752=CARTESIAN_POINT('Origin',(0.,-0.0492,0.));
#19753=CARTESIAN_POINT('',(-0.21,-0.02,-2.57175827820944E-17));
#19754=CARTESIAN_POINT('Origin',(0.,-0.8,0.));
#19755=CARTESIAN_POINT('',(-0.1954,-0.8,-2.39295984553393E-17));
#19756=CARTESIAN_POINT('',(0.,0.,0.));
#19757=CARTESIAN_POINT('',(0.,0.,0.));
#19758=CARTESIAN_POINT('Origin',(1.,0.,10.7));
#19759=CARTESIAN_POINT('',(0.575,-5.20474889637625E-17,10.8));
#19760=CARTESIAN_POINT('Origin',(1.,0.,10.8));
#19761=CARTESIAN_POINT('',(0.575,-5.20474889637625E-17,12.));
#19762=CARTESIAN_POINT('',(0.575,-5.20474889637625E-17,10.7));
#19763=CARTESIAN_POINT('Origin',(1.,0.,12.));
#19764=CARTESIAN_POINT('Origin',(1.,0.,12.));
#19765=CARTESIAN_POINT('Origin',(0.2,-1.,37.));
#19766=CARTESIAN_POINT('',(0.2,-0.6,37.));
#19767=CARTESIAN_POINT('',(0.2,-0.6,11.));
#19768=CARTESIAN_POINT('',(0.2,-0.6,10.8));
#19769=CARTESIAN_POINT('',(0.2,-1.,37.));
#19770=CARTESIAN_POINT('',(0.2,-1.,37.));
#19771=CARTESIAN_POINT('',(0.2,-1.,11.));
#19772=CARTESIAN_POINT('',(0.2,-1.,11.));
#19773=CARTESIAN_POINT('',(0.2,-1.,11.));
#19774=CARTESIAN_POINT('Origin',(0.2,-1.,37.));
#19775=CARTESIAN_POINT('',(0.2,0.6,11.));
#19776=CARTESIAN_POINT('',(0.2,0.6,37.));
#19777=CARTESIAN_POINT('',(0.2,0.6,10.8));
#19778=CARTESIAN_POINT('',(0.2,1.,11.));
#19779=CARTESIAN_POINT('',(0.2,-1.,11.));
#19780=CARTESIAN_POINT('',(0.2,1.,37.));
#19781=CARTESIAN_POINT('',(0.2,1.,11.));
#19782=CARTESIAN_POINT('',(0.2,-1.,37.));
#19783=CARTESIAN_POINT('Origin',(0.2,-1.,11.));
#19784=CARTESIAN_POINT('',(0.,-1.22464679914735E-16,11.));
#19785=CARTESIAN_POINT('Origin',(1.,0.,11.));
#19786=CARTESIAN_POINT('',(-1.,-1.,11.));
#19787=CARTESIAN_POINT('',(-1.,-1.,11.));
#19788=CARTESIAN_POINT('',(-1.,1.,11.));
#19789=CARTESIAN_POINT('',(-1.,-1.,11.));
#19790=CARTESIAN_POINT('',(-1.,1.,11.));
#19791=CARTESIAN_POINT('Origin',(1.,0.,11.));
#19792=CARTESIAN_POINT('Origin',(-1.,-1.,37.));
#19793=CARTESIAN_POINT('',(0.,-1.22464679914735E-16,37.));
#19794=CARTESIAN_POINT('Origin',(1.,0.,37.));
#19795=CARTESIAN_POINT('',(-1.,1.,37.));
#19796=CARTESIAN_POINT('',(0.2,1.,37.));
#19797=CARTESIAN_POINT('',(-1.,-1.,37.));
#19798=CARTESIAN_POINT('',(-1.,-1.,37.));
#19799=CARTESIAN_POINT('',(0.2,-1.,37.));
#19800=CARTESIAN_POINT('Origin',(1.,0.,37.));
#19801=CARTESIAN_POINT('Origin',(-1.,-1.,36.269194724554));
#19802=CARTESIAN_POINT('',(-1.,-1.,36.269194724554));
#19803=CARTESIAN_POINT('',(-1.,-1.,37.));
#19804=CARTESIAN_POINT('',(-1.,1.,36.269194724554));
#19805=CARTESIAN_POINT('',(-1.,1.,37.));
#19806=CARTESIAN_POINT('',(-1.,-1.,36.269194724554));
#19807=CARTESIAN_POINT('Origin',(-1.45,-1.,36.1054081191342));
#19808=CARTESIAN_POINT('',(-1.45,-1.,36.1054081191342));
#19809=CARTESIAN_POINT('',(-1.,-1.,36.269194724554));
#19810=CARTESIAN_POINT('',(-1.45,1.,36.1054081191342));
#19811=CARTESIAN_POINT('',(-1.,1.,36.269194724554));
#19812=CARTESIAN_POINT('',(-1.45,-1.,36.1054081191342));
#19813=CARTESIAN_POINT('Origin',(-1.45,-1.,35.9388369474817));
#19814=CARTESIAN_POINT('',(-1.45,-1.,35.9388369474817));
#19815=CARTESIAN_POINT('',(-1.45,-1.,36.1054081191342));
#19816=CARTESIAN_POINT('',(-1.45,1.,35.9388369474817));
#19817=CARTESIAN_POINT('',(-1.45,1.,36.1054081191342));
#19818=CARTESIAN_POINT('',(-1.45,-1.,35.9388369474817));
#19819=CARTESIAN_POINT('Origin',(-1.,-1.,35.7750503420619));
#19820=CARTESIAN_POINT('',(-1.,-1.,35.7750503420619));
#19821=CARTESIAN_POINT('',(-1.45,-1.,35.9388369474817));
#19822=CARTESIAN_POINT('',(-1.,1.,35.7750503420619));
#19823=CARTESIAN_POINT('',(-1.45,1.,35.9388369474817));
#19824=CARTESIAN_POINT('',(-1.,-1.,35.7750503420619));
#19825=CARTESIAN_POINT('Origin',(-1.,-1.,35.640876193836));
#19826=CARTESIAN_POINT('',(-1.,-1.,35.640876193836));
#19827=CARTESIAN_POINT('',(-1.,-1.,35.7750503420619));
#19828=CARTESIAN_POINT('',(-1.,1.,35.640876193836));
#19829=CARTESIAN_POINT('',(-1.,1.,35.7750503420619));
#19830=CARTESIAN_POINT('',(-1.,-1.,35.640876193836));
#19831=CARTESIAN_POINT('Origin',(-1.45,-1.,35.4770895884162));
#19832=CARTESIAN_POINT('',(-1.45,-1.,35.4770895884162));
#19833=CARTESIAN_POINT('',(-1.,-1.,35.640876193836));
#19834=CARTESIAN_POINT('',(-1.45,1.,35.4770895884162));
#19835=CARTESIAN_POINT('',(-1.,1.,35.640876193836));
#19836=CARTESIAN_POINT('',(-1.45,-1.,35.4770895884162));
#19837=CARTESIAN_POINT('Origin',(-1.45,-1.,35.3105184167637));
#19838=CARTESIAN_POINT('',(-1.45,-1.,35.3105184167637));
#19839=CARTESIAN_POINT('',(-1.45,-1.,35.4770895884162));
#19840=CARTESIAN_POINT('',(-1.45,1.,35.3105184167637));
#19841=CARTESIAN_POINT('',(-1.45,1.,35.4770895884162));
#19842=CARTESIAN_POINT('',(-1.45,-1.,35.3105184167637));
#19843=CARTESIAN_POINT('Origin',(-1.,-1.,35.1467318113439));
#19844=CARTESIAN_POINT('',(-1.,-1.,35.1467318113439));
#19845=CARTESIAN_POINT('',(-1.45,-1.,35.3105184167637));
#19846=CARTESIAN_POINT('',(-1.,1.,35.1467318113439));
#19847=CARTESIAN_POINT('',(-1.45,1.,35.3105184167637));
#19848=CARTESIAN_POINT('',(-1.,-1.,35.1467318113439));
#19849=CARTESIAN_POINT('Origin',(-1.,-1.,35.0125576631181));
#19850=CARTESIAN_POINT('',(-1.,-1.,35.0125576631181));
#19851=CARTESIAN_POINT('',(-1.,-1.,35.1467318113439));
#19852=CARTESIAN_POINT('',(-1.,1.,35.0125576631181));
#19853=CARTESIAN_POINT('',(-1.,1.,35.1467318113439));
#19854=CARTESIAN_POINT('',(-1.,-1.,35.0125576631181));
#19855=CARTESIAN_POINT('Origin',(-1.45,-1.,34.8487710576983));
#19856=CARTESIAN_POINT('',(-1.45,-1.,34.8487710576983));
#19857=CARTESIAN_POINT('',(-1.,-1.,35.0125576631181));
#19858=CARTESIAN_POINT('',(-1.45,1.,34.8487710576983));
#19859=CARTESIAN_POINT('',(-1.,1.,35.0125576631181));
#19860=CARTESIAN_POINT('',(-1.45,-1.,34.8487710576983));
#19861=CARTESIAN_POINT('Origin',(-1.45,-1.,34.6821998860458));
#19862=CARTESIAN_POINT('',(-1.45,-1.,34.6821998860458));
#19863=CARTESIAN_POINT('',(-1.45,-1.,34.8487710576983));
#19864=CARTESIAN_POINT('',(-1.45,1.,34.6821998860458));
#19865=CARTESIAN_POINT('',(-1.45,1.,34.8487710576983));
#19866=CARTESIAN_POINT('',(-1.45,-1.,34.6821998860458));
#19867=CARTESIAN_POINT('Origin',(-1.,-1.,34.518413280626));
#19868=CARTESIAN_POINT('',(-1.,-1.,34.518413280626));
#19869=CARTESIAN_POINT('',(-1.45,-1.,34.6821998860458));
#19870=CARTESIAN_POINT('',(-1.,1.,34.518413280626));
#19871=CARTESIAN_POINT('',(-1.45,1.,34.6821998860458));
#19872=CARTESIAN_POINT('',(-1.,-1.,34.518413280626));
#19873=CARTESIAN_POINT('Origin',(-1.,-1.,34.3842391324001));
#19874=CARTESIAN_POINT('',(-1.,-1.,34.3842391324001));
#19875=CARTESIAN_POINT('',(-1.,-1.,34.518413280626));
#19876=CARTESIAN_POINT('',(-1.,1.,34.3842391324001));
#19877=CARTESIAN_POINT('',(-1.,1.,34.518413280626));
#19878=CARTESIAN_POINT('',(-1.,-1.,34.3842391324001));
#19879=CARTESIAN_POINT('Origin',(-1.45,-1.,34.2204525269803));
#19880=CARTESIAN_POINT('',(-1.45,-1.,34.2204525269803));
#19881=CARTESIAN_POINT('',(-1.,-1.,34.3842391324001));
#19882=CARTESIAN_POINT('',(-1.45,1.,34.2204525269803));
#19883=CARTESIAN_POINT('',(-1.,1.,34.3842391324001));
#19884=CARTESIAN_POINT('',(-1.45,-1.,34.2204525269803));
#19885=CARTESIAN_POINT('Origin',(-1.45,-1.,34.0538813553278));
#19886=CARTESIAN_POINT('',(-1.45,-1.,34.0538813553278));
#19887=CARTESIAN_POINT('',(-1.45,-1.,34.2204525269803));
#19888=CARTESIAN_POINT('',(-1.45,1.,34.0538813553278));
#19889=CARTESIAN_POINT('',(-1.45,1.,34.2204525269803));
#19890=CARTESIAN_POINT('',(-1.45,-1.,34.0538813553278));
#19891=CARTESIAN_POINT('Origin',(-1.,-1.,33.890094749908));
#19892=CARTESIAN_POINT('',(-1.,-1.,33.890094749908));
#19893=CARTESIAN_POINT('',(-1.45,-1.,34.0538813553278));
#19894=CARTESIAN_POINT('',(-1.,1.,33.890094749908));
#19895=CARTESIAN_POINT('',(-1.45,1.,34.0538813553278));
#19896=CARTESIAN_POINT('',(-1.,-1.,33.890094749908));
#19897=CARTESIAN_POINT('Origin',(-1.,-1.,33.7559206016821));
#19898=CARTESIAN_POINT('',(-1.,-1.,33.7559206016821));
#19899=CARTESIAN_POINT('',(-1.,-1.,33.890094749908));
#19900=CARTESIAN_POINT('',(-1.,1.,33.7559206016821));
#19901=CARTESIAN_POINT('',(-1.,1.,33.890094749908));
#19902=CARTESIAN_POINT('',(-1.,-1.,33.7559206016821));
#19903=CARTESIAN_POINT('Origin',(-1.45,-1.,33.5921339962624));
#19904=CARTESIAN_POINT('',(-1.45,-1.,33.5921339962624));
#19905=CARTESIAN_POINT('',(-1.,-1.,33.7559206016821));
#19906=CARTESIAN_POINT('',(-1.45,1.,33.5921339962624));
#19907=CARTESIAN_POINT('',(-1.,1.,33.7559206016821));
#19908=CARTESIAN_POINT('',(-1.45,-1.,33.5921339962624));
#19909=CARTESIAN_POINT('Origin',(-1.45,-1.,33.4255628246099));
#19910=CARTESIAN_POINT('',(-1.45,-1.,33.4255628246099));
#19911=CARTESIAN_POINT('',(-1.45,-1.,33.5921339962624));
#19912=CARTESIAN_POINT('',(-1.45,1.,33.4255628246099));
#19913=CARTESIAN_POINT('',(-1.45,1.,33.5921339962624));
#19914=CARTESIAN_POINT('',(-1.45,-1.,33.4255628246099));
#19915=CARTESIAN_POINT('Origin',(-1.,-1.,33.2617762191901));
#19916=CARTESIAN_POINT('',(-1.,-1.,33.2617762191901));
#19917=CARTESIAN_POINT('',(-1.45,-1.,33.4255628246099));
#19918=CARTESIAN_POINT('',(-1.,1.,33.2617762191901));
#19919=CARTESIAN_POINT('',(-1.45,1.,33.4255628246099));
#19920=CARTESIAN_POINT('',(-1.,-1.,33.2617762191901));
#19921=CARTESIAN_POINT('Origin',(-1.,-1.,33.1276020709642));
#19922=CARTESIAN_POINT('',(-1.,-1.,33.1276020709642));
#19923=CARTESIAN_POINT('',(-1.,-1.,33.2617762191901));
#19924=CARTESIAN_POINT('',(-1.,1.,33.1276020709642));
#19925=CARTESIAN_POINT('',(-1.,1.,33.2617762191901));
#19926=CARTESIAN_POINT('',(-1.,-1.,33.1276020709642));
#19927=CARTESIAN_POINT('Origin',(-1.45,-1.,32.9638154655444));
#19928=CARTESIAN_POINT('',(-1.45,-1.,32.9638154655444));
#19929=CARTESIAN_POINT('',(-1.,-1.,33.1276020709642));
#19930=CARTESIAN_POINT('',(-1.45,1.,32.9638154655444));
#19931=CARTESIAN_POINT('',(-1.,1.,33.1276020709642));
#19932=CARTESIAN_POINT('',(-1.45,-1.,32.9638154655444));
#19933=CARTESIAN_POINT('Origin',(-1.45,-1.,32.7972442938919));
#19934=CARTESIAN_POINT('',(-1.45,-1.,32.7972442938919));
#19935=CARTESIAN_POINT('',(-1.45,-1.,32.9638154655444));
#19936=CARTESIAN_POINT('',(-1.45,1.,32.7972442938919));
#19937=CARTESIAN_POINT('',(-1.45,1.,32.9638154655444));
#19938=CARTESIAN_POINT('',(-1.45,-1.,32.7972442938919));
#19939=CARTESIAN_POINT('Origin',(-1.,-1.,32.6334576884721));
#19940=CARTESIAN_POINT('',(-1.,-1.,32.6334576884721));
#19941=CARTESIAN_POINT('',(-1.45,-1.,32.7972442938919));
#19942=CARTESIAN_POINT('',(-1.,1.,32.6334576884721));
#19943=CARTESIAN_POINT('',(-1.45,1.,32.7972442938919));
#19944=CARTESIAN_POINT('',(-1.,-1.,32.6334576884721));
#19945=CARTESIAN_POINT('Origin',(-1.,-1.,32.4992835402462));
#19946=CARTESIAN_POINT('',(-1.,-1.,32.4992835402462));
#19947=CARTESIAN_POINT('',(-1.,-1.,32.6334576884721));
#19948=CARTESIAN_POINT('',(-1.,1.,32.4992835402462));
#19949=CARTESIAN_POINT('',(-1.,1.,32.6334576884721));
#19950=CARTESIAN_POINT('',(-1.,-1.,32.4992835402462));
#19951=CARTESIAN_POINT('Origin',(-1.45,-1.,32.3354969348264));
#19952=CARTESIAN_POINT('',(-1.45,-1.,32.3354969348264));
#19953=CARTESIAN_POINT('',(-1.,-1.,32.4992835402462));
#19954=CARTESIAN_POINT('',(-1.45,1.,32.3354969348264));
#19955=CARTESIAN_POINT('',(-1.,1.,32.4992835402462));
#19956=CARTESIAN_POINT('',(-1.45,-1.,32.3354969348264));
#19957=CARTESIAN_POINT('Origin',(-1.45,-1.,32.1689257631739));
#19958=CARTESIAN_POINT('',(-1.45,-1.,32.1689257631739));
#19959=CARTESIAN_POINT('',(-1.45,-1.,32.3354969348264));
#19960=CARTESIAN_POINT('',(-1.45,1.,32.1689257631739));
#19961=CARTESIAN_POINT('',(-1.45,1.,32.3354969348264));
#19962=CARTESIAN_POINT('',(-1.45,-1.,32.1689257631739));
#19963=CARTESIAN_POINT('Origin',(-1.,-1.,32.0051391577542));
#19964=CARTESIAN_POINT('',(-1.,-1.,32.0051391577542));
#19965=CARTESIAN_POINT('',(-1.45,-1.,32.1689257631739));
#19966=CARTESIAN_POINT('',(-1.,1.,32.0051391577542));
#19967=CARTESIAN_POINT('',(-1.45,1.,32.1689257631739));
#19968=CARTESIAN_POINT('',(-1.,-1.,32.0051391577542));
#19969=CARTESIAN_POINT('Origin',(-1.,-1.,31.8709650095283));
#19970=CARTESIAN_POINT('',(-1.,-1.,31.8709650095283));
#19971=CARTESIAN_POINT('',(-1.,-1.,32.0051391577542));
#19972=CARTESIAN_POINT('',(-1.,1.,31.8709650095283));
#19973=CARTESIAN_POINT('',(-1.,1.,32.0051391577542));
#19974=CARTESIAN_POINT('',(-1.,-1.,31.8709650095283));
#19975=CARTESIAN_POINT('Origin',(-1.45,-1.,31.7071784041085));
#19976=CARTESIAN_POINT('',(-1.45,-1.,31.7071784041085));
#19977=CARTESIAN_POINT('',(-1.,-1.,31.8709650095283));
#19978=CARTESIAN_POINT('',(-1.45,1.,31.7071784041085));
#19979=CARTESIAN_POINT('',(-1.,1.,31.8709650095283));
#19980=CARTESIAN_POINT('',(-1.45,-1.,31.7071784041085));
#19981=CARTESIAN_POINT('Origin',(-1.45,-1.,31.540607232456));
#19982=CARTESIAN_POINT('',(-1.45,-1.,31.540607232456));
#19983=CARTESIAN_POINT('',(-1.45,-1.,31.7071784041085));
#19984=CARTESIAN_POINT('',(-1.45,1.,31.540607232456));
#19985=CARTESIAN_POINT('',(-1.45,1.,31.7071784041085));
#19986=CARTESIAN_POINT('',(-1.45,-1.,31.540607232456));
#19987=CARTESIAN_POINT('Origin',(-1.,-1.,31.3768206270362));
#19988=CARTESIAN_POINT('',(-1.,-1.,31.3768206270362));
#19989=CARTESIAN_POINT('',(-1.45,-1.,31.540607232456));
#19990=CARTESIAN_POINT('',(-1.,1.,31.3768206270362));
#19991=CARTESIAN_POINT('',(-1.45,1.,31.540607232456));
#19992=CARTESIAN_POINT('',(-1.,-1.,31.3768206270362));
#19993=CARTESIAN_POINT('Origin',(-1.,-1.,31.2426464788103));
#19994=CARTESIAN_POINT('',(-1.,-1.,31.2426464788103));
#19995=CARTESIAN_POINT('',(-1.,-1.,31.3768206270362));
#19996=CARTESIAN_POINT('',(-1.,1.,31.2426464788103));
#19997=CARTESIAN_POINT('',(-1.,1.,31.3768206270362));
#19998=CARTESIAN_POINT('',(-1.,-1.,31.2426464788103));
#19999=CARTESIAN_POINT('Origin',(-1.45,-1.,31.0788598733905));
#20000=CARTESIAN_POINT('',(-1.45,-1.,31.0788598733905));
#20001=CARTESIAN_POINT('',(-1.,-1.,31.2426464788103));
#20002=CARTESIAN_POINT('',(-1.45,1.,31.0788598733905));
#20003=CARTESIAN_POINT('',(-1.,1.,31.2426464788103));
#20004=CARTESIAN_POINT('',(-1.45,-1.,31.0788598733905));
#20005=CARTESIAN_POINT('Origin',(-1.45,-1.,30.912288701738));
#20006=CARTESIAN_POINT('',(-1.45,-1.,30.912288701738));
#20007=CARTESIAN_POINT('',(-1.45,-1.,31.0788598733905));
#20008=CARTESIAN_POINT('',(-1.45,1.,30.912288701738));
#20009=CARTESIAN_POINT('',(-1.45,1.,31.0788598733905));
#20010=CARTESIAN_POINT('',(-1.45,-1.,30.912288701738));
#20011=CARTESIAN_POINT('Origin',(-1.,-1.,30.7485020963182));
#20012=CARTESIAN_POINT('',(-1.,-1.,30.7485020963182));
#20013=CARTESIAN_POINT('',(-1.45,-1.,30.912288701738));
#20014=CARTESIAN_POINT('',(-1.,1.,30.7485020963182));
#20015=CARTESIAN_POINT('',(-1.45,1.,30.912288701738));
#20016=CARTESIAN_POINT('',(-1.,-1.,30.7485020963182));
#20017=CARTESIAN_POINT('Origin',(-1.,-1.,30.6143279480924));
#20018=CARTESIAN_POINT('',(-1.,-1.,30.6143279480924));
#20019=CARTESIAN_POINT('',(-1.,-1.,30.7485020963182));
#20020=CARTESIAN_POINT('',(-1.,1.,30.6143279480924));
#20021=CARTESIAN_POINT('',(-1.,1.,30.7485020963182));
#20022=CARTESIAN_POINT('',(-1.,-1.,30.6143279480924));
#20023=CARTESIAN_POINT('Origin',(-1.45,-1.,30.4505413426726));
#20024=CARTESIAN_POINT('',(-1.45,-1.,30.4505413426726));
#20025=CARTESIAN_POINT('',(-1.,-1.,30.6143279480924));
#20026=CARTESIAN_POINT('',(-1.45,1.,30.4505413426726));
#20027=CARTESIAN_POINT('',(-1.,1.,30.6143279480924));
#20028=CARTESIAN_POINT('',(-1.45,-1.,30.4505413426726));
#20029=CARTESIAN_POINT('Origin',(-1.45,-1.,30.2839701710201));
#20030=CARTESIAN_POINT('',(-1.45,-1.,30.2839701710201));
#20031=CARTESIAN_POINT('',(-1.45,-1.,30.4505413426726));
#20032=CARTESIAN_POINT('',(-1.45,1.,30.2839701710201));
#20033=CARTESIAN_POINT('',(-1.45,1.,30.4505413426726));
#20034=CARTESIAN_POINT('',(-1.45,-1.,30.2839701710201));
#20035=CARTESIAN_POINT('Origin',(-1.,-1.,30.1201835656003));
#20036=CARTESIAN_POINT('',(-1.,-1.,30.1201835656003));
#20037=CARTESIAN_POINT('',(-1.45,-1.,30.2839701710201));
#20038=CARTESIAN_POINT('',(-1.,1.,30.1201835656003));
#20039=CARTESIAN_POINT('',(-1.45,1.,30.2839701710201));
#20040=CARTESIAN_POINT('',(-1.,-1.,30.1201835656003));
#20041=CARTESIAN_POINT('Origin',(-1.,-1.,29.9860094173744));
#20042=CARTESIAN_POINT('',(-1.,-1.,29.9860094173744));
#20043=CARTESIAN_POINT('',(-1.,-1.,30.1201835656003));
#20044=CARTESIAN_POINT('',(-1.,1.,29.9860094173744));
#20045=CARTESIAN_POINT('',(-1.,1.,30.1201835656003));
#20046=CARTESIAN_POINT('',(-1.,-1.,29.9860094173744));
#20047=CARTESIAN_POINT('Origin',(-1.45,-1.,29.8222228119546));
#20048=CARTESIAN_POINT('',(-1.45,-1.,29.8222228119546));
#20049=CARTESIAN_POINT('',(-1.,-1.,29.9860094173744));
#20050=CARTESIAN_POINT('',(-1.45,1.,29.8222228119546));
#20051=CARTESIAN_POINT('',(-1.,1.,29.9860094173744));
#20052=CARTESIAN_POINT('',(-1.45,-1.,29.8222228119546));
#20053=CARTESIAN_POINT('Origin',(-1.45,-1.,29.6556516403021));
#20054=CARTESIAN_POINT('',(-1.45,-1.,29.6556516403021));
#20055=CARTESIAN_POINT('',(-1.45,-1.,29.8222228119546));
#20056=CARTESIAN_POINT('',(-1.45,1.,29.6556516403021));
#20057=CARTESIAN_POINT('',(-1.45,1.,29.8222228119546));
#20058=CARTESIAN_POINT('',(-1.45,-1.,29.6556516403021));
#20059=CARTESIAN_POINT('Origin',(-1.,-1.,29.4918650348823));
#20060=CARTESIAN_POINT('',(-1.,-1.,29.4918650348823));
#20061=CARTESIAN_POINT('',(-1.45,-1.,29.6556516403021));
#20062=CARTESIAN_POINT('',(-1.,1.,29.4918650348823));
#20063=CARTESIAN_POINT('',(-1.45,1.,29.6556516403021));
#20064=CARTESIAN_POINT('',(-1.,-1.,29.4918650348823));
#20065=CARTESIAN_POINT('Origin',(-1.,-1.,29.3576908866564));
#20066=CARTESIAN_POINT('',(-1.,-1.,29.3576908866564));
#20067=CARTESIAN_POINT('',(-1.,-1.,29.4918650348823));
#20068=CARTESIAN_POINT('',(-1.,1.,29.3576908866564));
#20069=CARTESIAN_POINT('',(-1.,1.,29.4918650348823));
#20070=CARTESIAN_POINT('',(-1.,-1.,29.3576908866564));
#20071=CARTESIAN_POINT('Origin',(-1.45,-1.,29.1939042812366));
#20072=CARTESIAN_POINT('',(-1.45,-1.,29.1939042812366));
#20073=CARTESIAN_POINT('',(-1.,-1.,29.3576908866564));
#20074=CARTESIAN_POINT('',(-1.45,1.,29.1939042812366));
#20075=CARTESIAN_POINT('',(-1.,1.,29.3576908866564));
#20076=CARTESIAN_POINT('',(-1.45,-1.,29.1939042812366));
#20077=CARTESIAN_POINT('Origin',(-1.45,-1.,29.0273331095841));
#20078=CARTESIAN_POINT('',(-1.45,-1.,29.0273331095841));
#20079=CARTESIAN_POINT('',(-1.45,-1.,29.1939042812366));
#20080=CARTESIAN_POINT('',(-1.45,1.,29.0273331095841));
#20081=CARTESIAN_POINT('',(-1.45,1.,29.1939042812366));
#20082=CARTESIAN_POINT('',(-1.45,-1.,29.0273331095841));
#20083=CARTESIAN_POINT('Origin',(-1.,-1.,28.8635465041644));
#20084=CARTESIAN_POINT('',(-1.,-1.,28.8635465041644));
#20085=CARTESIAN_POINT('',(-1.45,-1.,29.0273331095841));
#20086=CARTESIAN_POINT('',(-1.,1.,28.8635465041644));
#20087=CARTESIAN_POINT('',(-1.45,1.,29.0273331095841));
#20088=CARTESIAN_POINT('',(-1.,-1.,28.8635465041644));
#20089=CARTESIAN_POINT('Origin',(-1.,-1.,28.7293723559385));
#20090=CARTESIAN_POINT('',(-1.,-1.,28.7293723559385));
#20091=CARTESIAN_POINT('',(-1.,-1.,28.8635465041644));
#20092=CARTESIAN_POINT('',(-1.,1.,28.7293723559385));
#20093=CARTESIAN_POINT('',(-1.,1.,28.8635465041644));
#20094=CARTESIAN_POINT('',(-1.,-1.,28.7293723559385));
#20095=CARTESIAN_POINT('Origin',(-1.45,-1.,28.5655857505187));
#20096=CARTESIAN_POINT('',(-1.45,-1.,28.5655857505187));
#20097=CARTESIAN_POINT('',(-1.,-1.,28.7293723559385));
#20098=CARTESIAN_POINT('',(-1.45,1.,28.5655857505187));
#20099=CARTESIAN_POINT('',(-1.,1.,28.7293723559385));
#20100=CARTESIAN_POINT('',(-1.45,-1.,28.5655857505187));
#20101=CARTESIAN_POINT('Origin',(-1.45,-1.,28.3990145788662));
#20102=CARTESIAN_POINT('',(-1.45,-1.,28.3990145788662));
#20103=CARTESIAN_POINT('',(-1.45,-1.,28.5655857505187));
#20104=CARTESIAN_POINT('',(-1.45,1.,28.3990145788662));
#20105=CARTESIAN_POINT('',(-1.45,1.,28.5655857505187));
#20106=CARTESIAN_POINT('',(-1.45,-1.,28.3990145788662));
#20107=CARTESIAN_POINT('Origin',(-1.,-1.,28.2352279734464));
#20108=CARTESIAN_POINT('',(-1.,-1.,28.2352279734464));
#20109=CARTESIAN_POINT('',(-1.45,-1.,28.3990145788662));
#20110=CARTESIAN_POINT('',(-1.,1.,28.2352279734464));
#20111=CARTESIAN_POINT('',(-1.45,1.,28.3990145788662));
#20112=CARTESIAN_POINT('',(-1.,-1.,28.2352279734464));
#20113=CARTESIAN_POINT('Origin',(-1.,-1.,28.1010538252205));
#20114=CARTESIAN_POINT('',(-1.,-1.,28.1010538252205));
#20115=CARTESIAN_POINT('',(-1.,-1.,28.2352279734464));
#20116=CARTESIAN_POINT('',(-1.,1.,28.1010538252205));
#20117=CARTESIAN_POINT('',(-1.,1.,28.2352279734464));
#20118=CARTESIAN_POINT('',(-1.,-1.,28.1010538252205));
#20119=CARTESIAN_POINT('Origin',(-1.45,-1.,27.9372672198007));
#20120=CARTESIAN_POINT('',(-1.45,-1.,27.9372672198007));
#20121=CARTESIAN_POINT('',(-1.,-1.,28.1010538252205));
#20122=CARTESIAN_POINT('',(-1.45,1.,27.9372672198007));
#20123=CARTESIAN_POINT('',(-1.,1.,28.1010538252205));
#20124=CARTESIAN_POINT('',(-1.45,-1.,27.9372672198007));
#20125=CARTESIAN_POINT('Origin',(-1.45,-1.,27.7706960481482));
#20126=CARTESIAN_POINT('',(-1.45,-1.,27.7706960481482));
#20127=CARTESIAN_POINT('',(-1.45,-1.,27.9372672198007));
#20128=CARTESIAN_POINT('',(-1.45,1.,27.7706960481482));
#20129=CARTESIAN_POINT('',(-1.45,1.,27.9372672198007));
#20130=CARTESIAN_POINT('',(-1.45,-1.,27.7706960481482));
#20131=CARTESIAN_POINT('Origin',(-1.,-1.,27.6069094427284));
#20132=CARTESIAN_POINT('',(-1.,-1.,27.6069094427284));
#20133=CARTESIAN_POINT('',(-1.45,-1.,27.7706960481482));
#20134=CARTESIAN_POINT('',(-1.,1.,27.6069094427284));
#20135=CARTESIAN_POINT('',(-1.45,1.,27.7706960481482));
#20136=CARTESIAN_POINT('',(-1.,-1.,27.6069094427284));
#20137=CARTESIAN_POINT('Origin',(-1.,-1.,27.4727352945026));
#20138=CARTESIAN_POINT('',(-1.,-1.,27.4727352945026));
#20139=CARTESIAN_POINT('',(-1.,-1.,27.6069094427284));
#20140=CARTESIAN_POINT('',(-1.,1.,27.4727352945026));
#20141=CARTESIAN_POINT('',(-1.,1.,27.6069094427284));
#20142=CARTESIAN_POINT('',(-1.,-1.,27.4727352945026));
#20143=CARTESIAN_POINT('Origin',(-1.45,-1.,27.3089486890828));
#20144=CARTESIAN_POINT('',(-1.45,-1.,27.3089486890828));
#20145=CARTESIAN_POINT('',(-1.,-1.,27.4727352945026));
#20146=CARTESIAN_POINT('',(-1.45,1.,27.3089486890828));
#20147=CARTESIAN_POINT('',(-1.,1.,27.4727352945026));
#20148=CARTESIAN_POINT('',(-1.45,-1.,27.3089486890828));
#20149=CARTESIAN_POINT('Origin',(-1.45,-1.,27.1423775174303));
#20150=CARTESIAN_POINT('',(-1.45,-1.,27.1423775174303));
#20151=CARTESIAN_POINT('',(-1.45,-1.,27.3089486890828));
#20152=CARTESIAN_POINT('',(-1.45,1.,27.1423775174303));
#20153=CARTESIAN_POINT('',(-1.45,1.,27.3089486890828));
#20154=CARTESIAN_POINT('',(-1.45,-1.,27.1423775174303));
#20155=CARTESIAN_POINT('Origin',(-1.,-1.,26.9785909120105));
#20156=CARTESIAN_POINT('',(-1.,-1.,26.9785909120105));
#20157=CARTESIAN_POINT('',(-1.45,-1.,27.1423775174303));
#20158=CARTESIAN_POINT('',(-1.,1.,26.9785909120105));
#20159=CARTESIAN_POINT('',(-1.45,1.,27.1423775174303));
#20160=CARTESIAN_POINT('',(-1.,-1.,26.9785909120105));
#20161=CARTESIAN_POINT('Origin',(-1.,-1.,26.8444167637846));
#20162=CARTESIAN_POINT('',(-1.,-1.,26.8444167637846));
#20163=CARTESIAN_POINT('',(-1.,-1.,26.9785909120105));
#20164=CARTESIAN_POINT('',(-1.,1.,26.8444167637846));
#20165=CARTESIAN_POINT('',(-1.,1.,26.9785909120105));
#20166=CARTESIAN_POINT('',(-1.,-1.,26.8444167637846));
#20167=CARTESIAN_POINT('Origin',(-1.45,-1.,26.6806301583648));
#20168=CARTESIAN_POINT('',(-1.45,-1.,26.6806301583648));
#20169=CARTESIAN_POINT('',(-1.,-1.,26.8444167637846));
#20170=CARTESIAN_POINT('',(-1.45,1.,26.6806301583648));
#20171=CARTESIAN_POINT('',(-1.,1.,26.8444167637846));
#20172=CARTESIAN_POINT('',(-1.45,-1.,26.6806301583648));
#20173=CARTESIAN_POINT('Origin',(-1.45,-1.,26.5140589867123));
#20174=CARTESIAN_POINT('',(-1.45,-1.,26.5140589867123));
#20175=CARTESIAN_POINT('',(-1.45,-1.,26.6806301583648));
#20176=CARTESIAN_POINT('',(-1.45,1.,26.5140589867123));
#20177=CARTESIAN_POINT('',(-1.45,1.,26.6806301583648));
#20178=CARTESIAN_POINT('',(-1.45,-1.,26.5140589867123));
#20179=CARTESIAN_POINT('Origin',(-1.,-1.,26.3502723812925));
#20180=CARTESIAN_POINT('',(-1.,-1.,26.3502723812925));
#20181=CARTESIAN_POINT('',(-1.45,-1.,26.5140589867123));
#20182=CARTESIAN_POINT('',(-1.,1.,26.3502723812925));
#20183=CARTESIAN_POINT('',(-1.45,1.,26.5140589867123));
#20184=CARTESIAN_POINT('',(-1.,-1.,26.3502723812925));
#20185=CARTESIAN_POINT('Origin',(-1.,-1.,26.2160982330666));
#20186=CARTESIAN_POINT('',(-1.,-1.,26.2160982330666));
#20187=CARTESIAN_POINT('',(-1.,-1.,26.3502723812925));
#20188=CARTESIAN_POINT('',(-1.,1.,26.2160982330666));
#20189=CARTESIAN_POINT('',(-1.,1.,26.3502723812925));
#20190=CARTESIAN_POINT('',(-1.,-1.,26.2160982330666));
#20191=CARTESIAN_POINT('Origin',(-1.45,-1.,26.0523116276469));
#20192=CARTESIAN_POINT('',(-1.45,-1.,26.0523116276469));
#20193=CARTESIAN_POINT('',(-1.,-1.,26.2160982330666));
#20194=CARTESIAN_POINT('',(-1.45,1.,26.0523116276469));
#20195=CARTESIAN_POINT('',(-1.,1.,26.2160982330666));
#20196=CARTESIAN_POINT('',(-1.45,-1.,26.0523116276469));
#20197=CARTESIAN_POINT('Origin',(-1.45,-1.,25.8857404559944));
#20198=CARTESIAN_POINT('',(-1.45,-1.,25.8857404559944));
#20199=CARTESIAN_POINT('',(-1.45,-1.,26.0523116276469));
#20200=CARTESIAN_POINT('',(-1.45,1.,25.8857404559944));
#20201=CARTESIAN_POINT('',(-1.45,1.,26.0523116276469));
#20202=CARTESIAN_POINT('',(-1.45,-1.,25.8857404559944));
#20203=CARTESIAN_POINT('Origin',(-1.,-1.,25.7219538505746));
#20204=CARTESIAN_POINT('',(-1.,-1.,25.7219538505746));
#20205=CARTESIAN_POINT('',(-1.45,-1.,25.8857404559944));
#20206=CARTESIAN_POINT('',(-1.,1.,25.7219538505746));
#20207=CARTESIAN_POINT('',(-1.45,1.,25.8857404559944));
#20208=CARTESIAN_POINT('',(-1.,-1.,25.7219538505746));
#20209=CARTESIAN_POINT('Origin',(-1.,-1.,25.5877797023487));
#20210=CARTESIAN_POINT('',(-1.,-1.,25.5877797023487));
#20211=CARTESIAN_POINT('',(-1.,-1.,25.7219538505746));
#20212=CARTESIAN_POINT('',(-1.,1.,25.5877797023487));
#20213=CARTESIAN_POINT('',(-1.,1.,25.7219538505746));
#20214=CARTESIAN_POINT('',(-1.,-1.,25.5877797023487));
#20215=CARTESIAN_POINT('Origin',(-1.45,-1.,25.4239930969289));
#20216=CARTESIAN_POINT('',(-1.45,-1.,25.4239930969289));
#20217=CARTESIAN_POINT('',(-1.,-1.,25.5877797023487));
#20218=CARTESIAN_POINT('',(-1.45,1.,25.4239930969289));
#20219=CARTESIAN_POINT('',(-1.,1.,25.5877797023487));
#20220=CARTESIAN_POINT('',(-1.45,-1.,25.4239930969289));
#20221=CARTESIAN_POINT('Origin',(-1.45,-1.,25.2574219252764));
#20222=CARTESIAN_POINT('',(-1.45,-1.,25.2574219252764));
#20223=CARTESIAN_POINT('',(-1.45,-1.,25.4239930969289));
#20224=CARTESIAN_POINT('',(-1.45,1.,25.2574219252764));
#20225=CARTESIAN_POINT('',(-1.45,1.,25.4239930969289));
#20226=CARTESIAN_POINT('',(-1.45,-1.,25.2574219252764));
#20227=CARTESIAN_POINT('Origin',(-1.,-1.,25.0936353198566));
#20228=CARTESIAN_POINT('',(-1.,-1.,25.0936353198566));
#20229=CARTESIAN_POINT('',(-1.45,-1.,25.2574219252764));
#20230=CARTESIAN_POINT('',(-1.,1.,25.0936353198566));
#20231=CARTESIAN_POINT('',(-1.45,1.,25.2574219252764));
#20232=CARTESIAN_POINT('',(-1.,-1.,25.0936353198566));
#20233=CARTESIAN_POINT('Origin',(-1.,-1.,24.9594611716307));
#20234=CARTESIAN_POINT('',(-1.,-1.,24.9594611716307));
#20235=CARTESIAN_POINT('',(-1.,-1.,25.0936353198566));
#20236=CARTESIAN_POINT('',(-1.,1.,24.9594611716307));
#20237=CARTESIAN_POINT('',(-1.,1.,25.0936353198566));
#20238=CARTESIAN_POINT('',(-1.,-1.,24.9594611716307));
#20239=CARTESIAN_POINT('Origin',(-1.45,-1.,24.7956745662109));
#20240=CARTESIAN_POINT('',(-1.45,-1.,24.7956745662109));
#20241=CARTESIAN_POINT('',(-1.,-1.,24.9594611716307));
#20242=CARTESIAN_POINT('',(-1.45,1.,24.7956745662109));
#20243=CARTESIAN_POINT('',(-1.,1.,24.9594611716307));
#20244=CARTESIAN_POINT('',(-1.45,-1.,24.7956745662109));
#20245=CARTESIAN_POINT('Origin',(-1.45,-1.,24.6291033945584));
#20246=CARTESIAN_POINT('',(-1.45,-1.,24.6291033945584));
#20247=CARTESIAN_POINT('',(-1.45,-1.,24.7956745662109));
#20248=CARTESIAN_POINT('',(-1.45,1.,24.6291033945584));
#20249=CARTESIAN_POINT('',(-1.45,1.,24.7956745662109));
#20250=CARTESIAN_POINT('',(-1.45,-1.,24.6291033945584));
#20251=CARTESIAN_POINT('Origin',(-1.,-1.,24.4653167891386));
#20252=CARTESIAN_POINT('',(-1.,-1.,24.4653167891386));
#20253=CARTESIAN_POINT('',(-1.45,-1.,24.6291033945584));
#20254=CARTESIAN_POINT('',(-1.,1.,24.4653167891386));
#20255=CARTESIAN_POINT('',(-1.45,1.,24.6291033945584));
#20256=CARTESIAN_POINT('',(-1.,-1.,24.4653167891386));
#20257=CARTESIAN_POINT('Origin',(-1.,-1.,24.3311426409128));
#20258=CARTESIAN_POINT('',(-1.,-1.,24.3311426409128));
#20259=CARTESIAN_POINT('',(-1.,-1.,24.4653167891386));
#20260=CARTESIAN_POINT('',(-1.,1.,24.3311426409128));
#20261=CARTESIAN_POINT('',(-1.,1.,24.4653167891386));
#20262=CARTESIAN_POINT('',(-1.,-1.,24.3311426409128));
#20263=CARTESIAN_POINT('Origin',(-1.45,-1.,24.167356035493));
#20264=CARTESIAN_POINT('',(-1.45,-1.,24.167356035493));
#20265=CARTESIAN_POINT('',(-1.,-1.,24.3311426409128));
#20266=CARTESIAN_POINT('',(-1.45,1.,24.167356035493));
#20267=CARTESIAN_POINT('',(-1.,1.,24.3311426409128));
#20268=CARTESIAN_POINT('',(-1.45,-1.,24.167356035493));
#20269=CARTESIAN_POINT('Origin',(-1.45,-1.,24.0007848638405));
#20270=CARTESIAN_POINT('',(-1.45,-1.,24.0007848638405));
#20271=CARTESIAN_POINT('',(-1.45,-1.,24.167356035493));
#20272=CARTESIAN_POINT('',(-1.45,1.,24.0007848638405));
#20273=CARTESIAN_POINT('',(-1.45,1.,24.167356035493));
#20274=CARTESIAN_POINT('',(-1.45,-1.,24.0007848638405));
#20275=CARTESIAN_POINT('Origin',(-1.,-1.,23.8369982584207));
#20276=CARTESIAN_POINT('',(-1.,-1.,23.8369982584207));
#20277=CARTESIAN_POINT('',(-1.45,-1.,24.0007848638405));
#20278=CARTESIAN_POINT('',(-1.,1.,23.8369982584207));
#20279=CARTESIAN_POINT('',(-1.45,1.,24.0007848638405));
#20280=CARTESIAN_POINT('',(-1.,-1.,23.8369982584207));
#20281=CARTESIAN_POINT('Origin',(-1.,-1.,23.7028241101948));
#20282=CARTESIAN_POINT('',(-1.,-1.,23.7028241101948));
#20283=CARTESIAN_POINT('',(-1.,-1.,23.8369982584207));
#20284=CARTESIAN_POINT('',(-1.,1.,23.7028241101948));
#20285=CARTESIAN_POINT('',(-1.,1.,23.8369982584207));
#20286=CARTESIAN_POINT('',(-1.,-1.,23.7028241101948));
#20287=CARTESIAN_POINT('Origin',(-1.45,-1.,23.539037504775));
#20288=CARTESIAN_POINT('',(-1.45,-1.,23.539037504775));
#20289=CARTESIAN_POINT('',(-1.,-1.,23.7028241101948));
#20290=CARTESIAN_POINT('',(-1.45,1.,23.539037504775));
#20291=CARTESIAN_POINT('',(-1.,1.,23.7028241101948));
#20292=CARTESIAN_POINT('',(-1.45,-1.,23.539037504775));
#20293=CARTESIAN_POINT('Origin',(-1.45,-1.,23.3724663331225));
#20294=CARTESIAN_POINT('',(-1.45,-1.,23.3724663331225));
#20295=CARTESIAN_POINT('',(-1.45,-1.,23.539037504775));
#20296=CARTESIAN_POINT('',(-1.45,1.,23.3724663331225));
#20297=CARTESIAN_POINT('',(-1.45,1.,23.539037504775));
#20298=CARTESIAN_POINT('',(-1.45,-1.,23.3724663331225));
#20299=CARTESIAN_POINT('Origin',(-1.,-1.,23.2086797277027));
#20300=CARTESIAN_POINT('',(-1.,-1.,23.2086797277027));
#20301=CARTESIAN_POINT('',(-1.45,-1.,23.3724663331225));
#20302=CARTESIAN_POINT('',(-1.,1.,23.2086797277027));
#20303=CARTESIAN_POINT('',(-1.45,1.,23.3724663331225));
#20304=CARTESIAN_POINT('',(-1.,-1.,23.2086797277027));
#20305=CARTESIAN_POINT('Origin',(-1.,-1.,23.0745055794769));
#20306=CARTESIAN_POINT('',(-1.,-1.,23.0745055794769));
#20307=CARTESIAN_POINT('',(-1.,-1.,23.2086797277027));
#20308=CARTESIAN_POINT('',(-1.,1.,23.0745055794769));
#20309=CARTESIAN_POINT('',(-1.,1.,23.2086797277027));
#20310=CARTESIAN_POINT('',(-1.,-1.,23.0745055794769));
#20311=CARTESIAN_POINT('Origin',(-1.45,-1.,22.9107189740571));
#20312=CARTESIAN_POINT('',(-1.45,-1.,22.9107189740571));
#20313=CARTESIAN_POINT('',(-1.,-1.,23.0745055794769));
#20314=CARTESIAN_POINT('',(-1.45,1.,22.9107189740571));
#20315=CARTESIAN_POINT('',(-1.,1.,23.0745055794769));
#20316=CARTESIAN_POINT('',(-1.45,-1.,22.9107189740571));
#20317=CARTESIAN_POINT('Origin',(-1.45,-1.,22.7441478024046));
#20318=CARTESIAN_POINT('',(-1.45,-1.,22.7441478024046));
#20319=CARTESIAN_POINT('',(-1.45,-1.,22.9107189740571));
#20320=CARTESIAN_POINT('',(-1.45,1.,22.7441478024046));
#20321=CARTESIAN_POINT('',(-1.45,1.,22.9107189740571));
#20322=CARTESIAN_POINT('',(-1.45,-1.,22.7441478024046));
#20323=CARTESIAN_POINT('Origin',(-1.,-1.,22.5803611969848));
#20324=CARTESIAN_POINT('',(-1.,-1.,22.5803611969848));
#20325=CARTESIAN_POINT('',(-1.45,-1.,22.7441478024046));
#20326=CARTESIAN_POINT('',(-1.,1.,22.5803611969848));
#20327=CARTESIAN_POINT('',(-1.45,1.,22.7441478024046));
#20328=CARTESIAN_POINT('',(-1.,-1.,22.5803611969848));
#20329=CARTESIAN_POINT('Origin',(-1.,-1.,22.4461870487589));
#20330=CARTESIAN_POINT('',(-1.,-1.,22.4461870487589));
#20331=CARTESIAN_POINT('',(-1.,-1.,22.5803611969848));
#20332=CARTESIAN_POINT('',(-1.,1.,22.4461870487589));
#20333=CARTESIAN_POINT('',(-1.,1.,22.5803611969848));
#20334=CARTESIAN_POINT('',(-1.,-1.,22.4461870487589));
#20335=CARTESIAN_POINT('Origin',(-1.45,-1.,22.2824004433391));
#20336=CARTESIAN_POINT('',(-1.45,-1.,22.2824004433391));
#20337=CARTESIAN_POINT('',(-1.,-1.,22.4461870487589));
#20338=CARTESIAN_POINT('',(-1.45,1.,22.2824004433391));
#20339=CARTESIAN_POINT('',(-1.,1.,22.4461870487589));
#20340=CARTESIAN_POINT('',(-1.45,-1.,22.2824004433391));
#20341=CARTESIAN_POINT('Origin',(-1.45,-1.,22.1158292716866));
#20342=CARTESIAN_POINT('',(-1.45,-1.,22.1158292716866));
#20343=CARTESIAN_POINT('',(-1.45,-1.,22.2824004433391));
#20344=CARTESIAN_POINT('',(-1.45,1.,22.1158292716866));
#20345=CARTESIAN_POINT('',(-1.45,1.,22.2824004433391));
#20346=CARTESIAN_POINT('',(-1.45,-1.,22.1158292716866));
#20347=CARTESIAN_POINT('Origin',(-1.,-1.,21.9520426662668));
#20348=CARTESIAN_POINT('',(-1.,-1.,21.9520426662668));
#20349=CARTESIAN_POINT('',(-1.45,-1.,22.1158292716866));
#20350=CARTESIAN_POINT('',(-1.,1.,21.9520426662668));
#20351=CARTESIAN_POINT('',(-1.45,1.,22.1158292716866));
#20352=CARTESIAN_POINT('',(-1.,-1.,21.9520426662668));
#20353=CARTESIAN_POINT('Origin',(-1.,-1.,21.8178685180409));
#20354=CARTESIAN_POINT('',(-1.,-1.,21.8178685180409));
#20355=CARTESIAN_POINT('',(-1.,-1.,21.9520426662668));
#20356=CARTESIAN_POINT('',(-1.,1.,21.8178685180409));
#20357=CARTESIAN_POINT('',(-1.,1.,21.9520426662668));
#20358=CARTESIAN_POINT('',(-1.,-1.,21.8178685180409));
#20359=CARTESIAN_POINT('Origin',(-1.45,-1.,21.6540819126211));
#20360=CARTESIAN_POINT('',(-1.45,-1.,21.6540819126211));
#20361=CARTESIAN_POINT('',(-1.,-1.,21.8178685180409));
#20362=CARTESIAN_POINT('',(-1.45,1.,21.6540819126211));
#20363=CARTESIAN_POINT('',(-1.,1.,21.8178685180409));
#20364=CARTESIAN_POINT('',(-1.45,-1.,21.6540819126211));
#20365=CARTESIAN_POINT('Origin',(-1.45,-1.,21.4875107409686));
#20366=CARTESIAN_POINT('',(-1.45,-1.,21.4875107409686));
#20367=CARTESIAN_POINT('',(-1.45,-1.,21.6540819126211));
#20368=CARTESIAN_POINT('',(-1.45,1.,21.4875107409686));
#20369=CARTESIAN_POINT('',(-1.45,1.,21.6540819126211));
#20370=CARTESIAN_POINT('',(-1.45,-1.,21.4875107409686));
#20371=CARTESIAN_POINT('Origin',(-1.,-1.,21.3237241355489));
#20372=CARTESIAN_POINT('',(-1.,-1.,21.3237241355489));
#20373=CARTESIAN_POINT('',(-1.45,-1.,21.4875107409686));
#20374=CARTESIAN_POINT('',(-1.,1.,21.3237241355489));
#20375=CARTESIAN_POINT('',(-1.45,1.,21.4875107409686));
#20376=CARTESIAN_POINT('',(-1.,-1.,21.3237241355489));
#20377=CARTESIAN_POINT('Origin',(-1.,-1.,21.189549987323));
#20378=CARTESIAN_POINT('',(-1.,-1.,21.189549987323));
#20379=CARTESIAN_POINT('',(-1.,-1.,21.3237241355489));
#20380=CARTESIAN_POINT('',(-1.,1.,21.189549987323));
#20381=CARTESIAN_POINT('',(-1.,1.,21.3237241355489));
#20382=CARTESIAN_POINT('',(-1.,-1.,21.189549987323));
#20383=CARTESIAN_POINT('Origin',(-1.45,-1.,21.0257633819032));
#20384=CARTESIAN_POINT('',(-1.45,-1.,21.0257633819032));
#20385=CARTESIAN_POINT('',(-1.,-1.,21.189549987323));
#20386=CARTESIAN_POINT('',(-1.45,1.,21.0257633819032));
#20387=CARTESIAN_POINT('',(-1.,1.,21.189549987323));
#20388=CARTESIAN_POINT('',(-1.45,-1.,21.0257633819032));
#20389=CARTESIAN_POINT('Origin',(-1.45,-1.,20.8591922102507));
#20390=CARTESIAN_POINT('',(-1.45,-1.,20.8591922102507));
#20391=CARTESIAN_POINT('',(-1.45,-1.,21.0257633819032));
#20392=CARTESIAN_POINT('',(-1.45,1.,20.8591922102507));
#20393=CARTESIAN_POINT('',(-1.45,1.,21.0257633819032));
#20394=CARTESIAN_POINT('',(-1.45,-1.,20.8591922102507));
#20395=CARTESIAN_POINT('Origin',(-1.,-1.,20.6954056048309));
#20396=CARTESIAN_POINT('',(-1.,-1.,20.6954056048309));
#20397=CARTESIAN_POINT('',(-1.45,-1.,20.8591922102507));
#20398=CARTESIAN_POINT('',(-1.,1.,20.6954056048309));
#20399=CARTESIAN_POINT('',(-1.45,1.,20.8591922102507));
#20400=CARTESIAN_POINT('',(-1.,-1.,20.6954056048309));
#20401=CARTESIAN_POINT('Origin',(-1.,-1.,20.561231456605));
#20402=CARTESIAN_POINT('',(-1.,-1.,20.561231456605));
#20403=CARTESIAN_POINT('',(-1.,-1.,20.6954056048309));
#20404=CARTESIAN_POINT('',(-1.,1.,20.561231456605));
#20405=CARTESIAN_POINT('',(-1.,1.,20.6954056048309));
#20406=CARTESIAN_POINT('',(-1.,-1.,20.561231456605));
#20407=CARTESIAN_POINT('Origin',(-1.45,-1.,20.3974448511852));
#20408=CARTESIAN_POINT('',(-1.45,-1.,20.3974448511852));
#20409=CARTESIAN_POINT('',(-1.,-1.,20.561231456605));
#20410=CARTESIAN_POINT('',(-1.45,1.,20.3974448511852));
#20411=CARTESIAN_POINT('',(-1.,1.,20.561231456605));
#20412=CARTESIAN_POINT('',(-1.45,-1.,20.3974448511852));
#20413=CARTESIAN_POINT('Origin',(-1.45,-1.,20.2308736795327));
#20414=CARTESIAN_POINT('',(-1.45,-1.,20.2308736795327));
#20415=CARTESIAN_POINT('',(-1.45,-1.,20.3974448511852));
#20416=CARTESIAN_POINT('',(-1.45,1.,20.2308736795327));
#20417=CARTESIAN_POINT('',(-1.45,1.,20.3974448511852));
#20418=CARTESIAN_POINT('',(-1.45,-1.,20.2308736795327));
#20419=CARTESIAN_POINT('Origin',(-1.,-1.,20.0670870741129));
#20420=CARTESIAN_POINT('',(-1.,-1.,20.0670870741129));
#20421=CARTESIAN_POINT('',(-1.45,-1.,20.2308736795327));
#20422=CARTESIAN_POINT('',(-1.,1.,20.0670870741129));
#20423=CARTESIAN_POINT('',(-1.45,1.,20.2308736795327));
#20424=CARTESIAN_POINT('',(-1.,-1.,20.0670870741129));
#20425=CARTESIAN_POINT('Origin',(-1.,-1.,19.9329129258871));
#20426=CARTESIAN_POINT('',(-1.,-1.,19.9329129258871));
#20427=CARTESIAN_POINT('',(-1.,-1.,20.0670870741129));
#20428=CARTESIAN_POINT('',(-1.,1.,19.9329129258871));
#20429=CARTESIAN_POINT('',(-1.,1.,20.0670870741129));
#20430=CARTESIAN_POINT('',(-1.,-1.,19.9329129258871));
#20431=CARTESIAN_POINT('Origin',(-1.45,-1.,19.7691263204673));
#20432=CARTESIAN_POINT('',(-1.45,-1.,19.7691263204673));
#20433=CARTESIAN_POINT('',(-1.,-1.,19.9329129258871));
#20434=CARTESIAN_POINT('',(-1.45,1.,19.7691263204673));
#20435=CARTESIAN_POINT('',(-1.,1.,19.9329129258871));
#20436=CARTESIAN_POINT('',(-1.45,-1.,19.7691263204673));
#20437=CARTESIAN_POINT('Origin',(-1.45,-1.,19.6025551488148));
#20438=CARTESIAN_POINT('',(-1.45,-1.,19.6025551488148));
#20439=CARTESIAN_POINT('',(-1.45,-1.,19.7691263204673));
#20440=CARTESIAN_POINT('',(-1.45,1.,19.6025551488148));
#20441=CARTESIAN_POINT('',(-1.45,1.,19.7691263204673));
#20442=CARTESIAN_POINT('',(-1.45,-1.,19.6025551488148));
#20443=CARTESIAN_POINT('Origin',(-1.,-1.,19.438768543395));
#20444=CARTESIAN_POINT('',(-1.,-1.,19.438768543395));
#20445=CARTESIAN_POINT('',(-1.45,-1.,19.6025551488148));
#20446=CARTESIAN_POINT('',(-1.,1.,19.438768543395));
#20447=CARTESIAN_POINT('',(-1.45,1.,19.6025551488148));
#20448=CARTESIAN_POINT('',(-1.,-1.,19.438768543395));
#20449=CARTESIAN_POINT('Origin',(-1.,-1.,19.3045943951691));
#20450=CARTESIAN_POINT('',(-1.,-1.,19.3045943951691));
#20451=CARTESIAN_POINT('',(-1.,-1.,19.438768543395));
#20452=CARTESIAN_POINT('',(-1.,1.,19.3045943951691));
#20453=CARTESIAN_POINT('',(-1.,1.,19.438768543395));
#20454=CARTESIAN_POINT('',(-1.,-1.,19.3045943951691));
#20455=CARTESIAN_POINT('Origin',(-1.45,-1.,19.1408077897493));
#20456=CARTESIAN_POINT('',(-1.45,-1.,19.1408077897493));
#20457=CARTESIAN_POINT('',(-1.,-1.,19.3045943951691));
#20458=CARTESIAN_POINT('',(-1.45,1.,19.1408077897493));
#20459=CARTESIAN_POINT('',(-1.,1.,19.3045943951691));
#20460=CARTESIAN_POINT('',(-1.45,-1.,19.1408077897493));
#20461=CARTESIAN_POINT('Origin',(-1.45,-1.,18.9742366180968));
#20462=CARTESIAN_POINT('',(-1.45,-1.,18.9742366180968));
#20463=CARTESIAN_POINT('',(-1.45,-1.,19.1408077897493));
#20464=CARTESIAN_POINT('',(-1.45,1.,18.9742366180968));
#20465=CARTESIAN_POINT('',(-1.45,1.,19.1408077897493));
#20466=CARTESIAN_POINT('',(-1.45,-1.,18.9742366180968));
#20467=CARTESIAN_POINT('Origin',(-1.,-1.,18.810450012677));
#20468=CARTESIAN_POINT('',(-1.,-1.,18.810450012677));
#20469=CARTESIAN_POINT('',(-1.45,-1.,18.9742366180968));
#20470=CARTESIAN_POINT('',(-1.,1.,18.810450012677));
#20471=CARTESIAN_POINT('',(-1.45,1.,18.9742366180968));
#20472=CARTESIAN_POINT('',(-1.,-1.,18.810450012677));
#20473=CARTESIAN_POINT('Origin',(-1.,-1.,18.6762758644511));
#20474=CARTESIAN_POINT('',(-1.,-1.,18.6762758644511));
#20475=CARTESIAN_POINT('',(-1.,-1.,18.810450012677));
#20476=CARTESIAN_POINT('',(-1.,1.,18.6762758644511));
#20477=CARTESIAN_POINT('',(-1.,1.,18.810450012677));
#20478=CARTESIAN_POINT('',(-1.,-1.,18.6762758644511));
#20479=CARTESIAN_POINT('Origin',(-1.45,-1.,18.5124892590314));
#20480=CARTESIAN_POINT('',(-1.45,-1.,18.5124892590314));
#20481=CARTESIAN_POINT('',(-1.,-1.,18.6762758644511));
#20482=CARTESIAN_POINT('',(-1.45,1.,18.5124892590314));
#20483=CARTESIAN_POINT('',(-1.,1.,18.6762758644511));
#20484=CARTESIAN_POINT('',(-1.45,-1.,18.5124892590314));
#20485=CARTESIAN_POINT('Origin',(-1.45,-1.,18.3459180873789));
#20486=CARTESIAN_POINT('',(-1.45,-1.,18.3459180873789));
#20487=CARTESIAN_POINT('',(-1.45,-1.,18.5124892590314));
#20488=CARTESIAN_POINT('',(-1.45,1.,18.3459180873789));
#20489=CARTESIAN_POINT('',(-1.45,1.,18.5124892590314));
#20490=CARTESIAN_POINT('',(-1.45,-1.,18.3459180873789));
#20491=CARTESIAN_POINT('Origin',(-1.,-1.,18.1821314819591));
#20492=CARTESIAN_POINT('',(-1.,-1.,18.1821314819591));
#20493=CARTESIAN_POINT('',(-1.45,-1.,18.3459180873789));
#20494=CARTESIAN_POINT('',(-1.,1.,18.1821314819591));
#20495=CARTESIAN_POINT('',(-1.45,1.,18.3459180873789));
#20496=CARTESIAN_POINT('',(-1.,-1.,18.1821314819591));
#20497=CARTESIAN_POINT('Origin',(-1.,-1.,18.0479573337332));
#20498=CARTESIAN_POINT('',(-1.,-1.,18.0479573337332));
#20499=CARTESIAN_POINT('',(-1.,-1.,18.1821314819591));
#20500=CARTESIAN_POINT('',(-1.,1.,18.0479573337332));
#20501=CARTESIAN_POINT('',(-1.,1.,18.1821314819591));
#20502=CARTESIAN_POINT('',(-1.,-1.,18.0479573337332));
#20503=CARTESIAN_POINT('Origin',(-1.45,-1.,17.8841707283134));
#20504=CARTESIAN_POINT('',(-1.45,-1.,17.8841707283134));
#20505=CARTESIAN_POINT('',(-1.,-1.,18.0479573337332));
#20506=CARTESIAN_POINT('',(-1.45,1.,17.8841707283134));
#20507=CARTESIAN_POINT('',(-1.,1.,18.0479573337332));
#20508=CARTESIAN_POINT('',(-1.45,-1.,17.8841707283134));
#20509=CARTESIAN_POINT('Origin',(-1.45,-1.,17.7175995566609));
#20510=CARTESIAN_POINT('',(-1.45,-1.,17.7175995566609));
#20511=CARTESIAN_POINT('',(-1.45,-1.,17.8841707283134));
#20512=CARTESIAN_POINT('',(-1.45,1.,17.7175995566609));
#20513=CARTESIAN_POINT('',(-1.45,1.,17.8841707283134));
#20514=CARTESIAN_POINT('',(-1.45,-1.,17.7175995566609));
#20515=CARTESIAN_POINT('Origin',(-1.,-1.,17.5538129512411));
#20516=CARTESIAN_POINT('',(-1.,-1.,17.5538129512411));
#20517=CARTESIAN_POINT('',(-1.45,-1.,17.7175995566609));
#20518=CARTESIAN_POINT('',(-1.,1.,17.5538129512411));
#20519=CARTESIAN_POINT('',(-1.45,1.,17.7175995566609));
#20520=CARTESIAN_POINT('',(-1.,-1.,17.5538129512411));
#20521=CARTESIAN_POINT('Origin',(-1.,-1.,17.4196388030152));
#20522=CARTESIAN_POINT('',(-1.,-1.,17.4196388030152));
#20523=CARTESIAN_POINT('',(-1.,-1.,17.5538129512411));
#20524=CARTESIAN_POINT('',(-1.,1.,17.4196388030152));
#20525=CARTESIAN_POINT('',(-1.,1.,17.5538129512411));
#20526=CARTESIAN_POINT('',(-1.,-1.,17.4196388030152));
#20527=CARTESIAN_POINT('Origin',(-1.45,-1.,17.2558521975954));
#20528=CARTESIAN_POINT('',(-1.45,-1.,17.2558521975954));
#20529=CARTESIAN_POINT('',(-1.,-1.,17.4196388030152));
#20530=CARTESIAN_POINT('',(-1.45,1.,17.2558521975954));
#20531=CARTESIAN_POINT('',(-1.,1.,17.4196388030152));
#20532=CARTESIAN_POINT('',(-1.45,-1.,17.2558521975954));
#20533=CARTESIAN_POINT('Origin',(-1.45,-1.,17.0892810259429));
#20534=CARTESIAN_POINT('',(-1.45,-1.,17.0892810259429));
#20535=CARTESIAN_POINT('',(-1.45,-1.,17.2558521975954));
#20536=CARTESIAN_POINT('',(-1.45,1.,17.0892810259429));
#20537=CARTESIAN_POINT('',(-1.45,1.,17.2558521975954));
#20538=CARTESIAN_POINT('',(-1.45,-1.,17.0892810259429));
#20539=CARTESIAN_POINT('Origin',(-1.,-1.,16.9254944205231));
#20540=CARTESIAN_POINT('',(-1.,-1.,16.9254944205231));
#20541=CARTESIAN_POINT('',(-1.45,-1.,17.0892810259429));
#20542=CARTESIAN_POINT('',(-1.,1.,16.9254944205231));
#20543=CARTESIAN_POINT('',(-1.45,1.,17.0892810259429));
#20544=CARTESIAN_POINT('',(-1.,-1.,16.9254944205231));
#20545=CARTESIAN_POINT('Origin',(-1.,-1.,16.7913202722973));
#20546=CARTESIAN_POINT('',(-1.,-1.,16.7913202722973));
#20547=CARTESIAN_POINT('',(-1.,-1.,16.9254944205231));
#20548=CARTESIAN_POINT('',(-1.,1.,16.7913202722973));
#20549=CARTESIAN_POINT('',(-1.,1.,16.9254944205231));
#20550=CARTESIAN_POINT('',(-1.,-1.,16.7913202722973));
#20551=CARTESIAN_POINT('Origin',(-1.45,-1.,16.6275336668775));
#20552=CARTESIAN_POINT('',(-1.45,-1.,16.6275336668775));
#20553=CARTESIAN_POINT('',(-1.,-1.,16.7913202722973));
#20554=CARTESIAN_POINT('',(-1.45,1.,16.6275336668775));
#20555=CARTESIAN_POINT('',(-1.,1.,16.7913202722973));
#20556=CARTESIAN_POINT('',(-1.45,-1.,16.6275336668775));
#20557=CARTESIAN_POINT('Origin',(-1.45,-1.,16.460962495225));
#20558=CARTESIAN_POINT('',(-1.45,-1.,16.460962495225));
#20559=CARTESIAN_POINT('',(-1.45,-1.,16.6275336668775));
#20560=CARTESIAN_POINT('',(-1.45,1.,16.460962495225));
#20561=CARTESIAN_POINT('',(-1.45,1.,16.6275336668775));
#20562=CARTESIAN_POINT('',(-1.45,-1.,16.460962495225));
#20563=CARTESIAN_POINT('Origin',(-1.,-1.,16.2971758898052));
#20564=CARTESIAN_POINT('',(-1.,-1.,16.2971758898052));
#20565=CARTESIAN_POINT('',(-1.45,-1.,16.460962495225));
#20566=CARTESIAN_POINT('',(-1.,1.,16.2971758898052));
#20567=CARTESIAN_POINT('',(-1.45,1.,16.460962495225));
#20568=CARTESIAN_POINT('',(-1.,-1.,16.2971758898052));
#20569=CARTESIAN_POINT('Origin',(-1.,-1.,16.1630017415793));
#20570=CARTESIAN_POINT('',(-1.,-1.,16.1630017415793));
#20571=CARTESIAN_POINT('',(-1.,-1.,16.2971758898052));
#20572=CARTESIAN_POINT('',(-1.,1.,16.1630017415793));
#20573=CARTESIAN_POINT('',(-1.,1.,16.2971758898052));
#20574=CARTESIAN_POINT('',(-1.,-1.,16.1630017415793));
#20575=CARTESIAN_POINT('Origin',(-1.45,-1.,15.9992151361595));
#20576=CARTESIAN_POINT('',(-1.45,-1.,15.9992151361595));
#20577=CARTESIAN_POINT('',(-1.,-1.,16.1630017415793));
#20578=CARTESIAN_POINT('',(-1.45,1.,15.9992151361595));
#20579=CARTESIAN_POINT('',(-1.,1.,16.1630017415793));
#20580=CARTESIAN_POINT('',(-1.45,-1.,15.9992151361595));
#20581=CARTESIAN_POINT('Origin',(-1.45,-1.,15.832643964507));
#20582=CARTESIAN_POINT('',(-1.45,-1.,15.832643964507));
#20583=CARTESIAN_POINT('',(-1.45,-1.,15.9992151361595));
#20584=CARTESIAN_POINT('',(-1.45,1.,15.832643964507));
#20585=CARTESIAN_POINT('',(-1.45,1.,15.9992151361595));
#20586=CARTESIAN_POINT('',(-1.45,-1.,15.832643964507));
#20587=CARTESIAN_POINT('Origin',(-1.,-1.,15.6688573590872));
#20588=CARTESIAN_POINT('',(-1.,-1.,15.6688573590872));
#20589=CARTESIAN_POINT('',(-1.45,-1.,15.832643964507));
#20590=CARTESIAN_POINT('',(-1.,1.,15.6688573590872));
#20591=CARTESIAN_POINT('',(-1.45,1.,15.832643964507));
#20592=CARTESIAN_POINT('',(-1.,-1.,15.6688573590872));
#20593=CARTESIAN_POINT('Origin',(-1.,-1.,15.5346832108613));
#20594=CARTESIAN_POINT('',(-1.,-1.,15.5346832108613));
#20595=CARTESIAN_POINT('',(-1.,-1.,15.6688573590872));
#20596=CARTESIAN_POINT('',(-1.,1.,15.5346832108613));
#20597=CARTESIAN_POINT('',(-1.,1.,15.6688573590872));
#20598=CARTESIAN_POINT('',(-1.,-1.,15.5346832108613));
#20599=CARTESIAN_POINT('Origin',(-1.45,-1.,15.3708966054416));
#20600=CARTESIAN_POINT('',(-1.45,-1.,15.3708966054416));
#20601=CARTESIAN_POINT('',(-1.,-1.,15.5346832108613));
#20602=CARTESIAN_POINT('',(-1.45,1.,15.3708966054416));
#20603=CARTESIAN_POINT('',(-1.,1.,15.5346832108613));
#20604=CARTESIAN_POINT('',(-1.45,-1.,15.3708966054416));
#20605=CARTESIAN_POINT('Origin',(-1.45,-1.,15.2043254337891));
#20606=CARTESIAN_POINT('',(-1.45,-1.,15.2043254337891));
#20607=CARTESIAN_POINT('',(-1.45,-1.,15.3708966054416));
#20608=CARTESIAN_POINT('',(-1.45,1.,15.2043254337891));
#20609=CARTESIAN_POINT('',(-1.45,1.,15.3708966054416));
#20610=CARTESIAN_POINT('',(-1.45,-1.,15.2043254337891));
#20611=CARTESIAN_POINT('Origin',(-1.,-1.,15.0405388283693));
#20612=CARTESIAN_POINT('',(-1.,-1.,15.0405388283693));
#20613=CARTESIAN_POINT('',(-1.45,-1.,15.2043254337891));
#20614=CARTESIAN_POINT('',(-1.,1.,15.0405388283693));
#20615=CARTESIAN_POINT('',(-1.45,1.,15.2043254337891));
#20616=CARTESIAN_POINT('',(-1.,-1.,15.0405388283693));
#20617=CARTESIAN_POINT('Origin',(-1.,-1.,14.9063646801434));
#20618=CARTESIAN_POINT('',(-1.,-1.,14.9063646801434));
#20619=CARTESIAN_POINT('',(-1.,-1.,15.0405388283693));
#20620=CARTESIAN_POINT('',(-1.,1.,14.9063646801434));
#20621=CARTESIAN_POINT('',(-1.,1.,15.0405388283693));
#20622=CARTESIAN_POINT('',(-1.,-1.,14.9063646801434));
#20623=CARTESIAN_POINT('Origin',(-1.45,-1.,14.7425780747236));
#20624=CARTESIAN_POINT('',(-1.45,-1.,14.7425780747236));
#20625=CARTESIAN_POINT('',(-1.,-1.,14.9063646801434));
#20626=CARTESIAN_POINT('',(-1.45,1.,14.7425780747236));
#20627=CARTESIAN_POINT('',(-1.,1.,14.9063646801434));
#20628=CARTESIAN_POINT('',(-1.45,-1.,14.7425780747236));
#20629=CARTESIAN_POINT('Origin',(-1.45,-1.,14.5760069030711));
#20630=CARTESIAN_POINT('',(-1.45,-1.,14.5760069030711));
#20631=CARTESIAN_POINT('',(-1.45,-1.,14.7425780747236));
#20632=CARTESIAN_POINT('',(-1.45,1.,14.5760069030711));
#20633=CARTESIAN_POINT('',(-1.45,1.,14.7425780747236));
#20634=CARTESIAN_POINT('',(-1.45,-1.,14.5760069030711));
#20635=CARTESIAN_POINT('Origin',(-1.,-1.,14.4122202976513));
#20636=CARTESIAN_POINT('',(-1.,-1.,14.4122202976513));
#20637=CARTESIAN_POINT('',(-1.45,-1.,14.5760069030711));
#20638=CARTESIAN_POINT('',(-1.,1.,14.4122202976513));
#20639=CARTESIAN_POINT('',(-1.45,1.,14.5760069030711));
#20640=CARTESIAN_POINT('',(-1.,-1.,14.4122202976513));
#20641=CARTESIAN_POINT('Origin',(-1.,-1.,14.2780461494254));
#20642=CARTESIAN_POINT('',(-1.,-1.,14.2780461494254));
#20643=CARTESIAN_POINT('',(-1.,-1.,14.4122202976513));
#20644=CARTESIAN_POINT('',(-1.,1.,14.2780461494254));
#20645=CARTESIAN_POINT('',(-1.,1.,14.4122202976513));
#20646=CARTESIAN_POINT('',(-1.,-1.,14.2780461494254));
#20647=CARTESIAN_POINT('Origin',(-1.45,-1.,14.1142595440056));
#20648=CARTESIAN_POINT('',(-1.45,-1.,14.1142595440056));
#20649=CARTESIAN_POINT('',(-1.,-1.,14.2780461494254));
#20650=CARTESIAN_POINT('',(-1.45,1.,14.1142595440056));
#20651=CARTESIAN_POINT('',(-1.,1.,14.2780461494254));
#20652=CARTESIAN_POINT('',(-1.45,-1.,14.1142595440056));
#20653=CARTESIAN_POINT('Origin',(-1.45,-1.,13.9476883723531));
#20654=CARTESIAN_POINT('',(-1.45,-1.,13.9476883723531));
#20655=CARTESIAN_POINT('',(-1.45,-1.,14.1142595440056));
#20656=CARTESIAN_POINT('',(-1.45,1.,13.9476883723531));
#20657=CARTESIAN_POINT('',(-1.45,1.,14.1142595440056));
#20658=CARTESIAN_POINT('',(-1.45,-1.,13.9476883723531));
#20659=CARTESIAN_POINT('Origin',(-1.,-1.,13.7839017669334));
#20660=CARTESIAN_POINT('',(-1.,-1.,13.7839017669334));
#20661=CARTESIAN_POINT('',(-1.45,-1.,13.9476883723531));
#20662=CARTESIAN_POINT('',(-1.,1.,13.7839017669334));
#20663=CARTESIAN_POINT('',(-1.45,1.,13.9476883723531));
#20664=CARTESIAN_POINT('',(-1.,-1.,13.7839017669334));
#20665=CARTESIAN_POINT('Origin',(-1.,-1.,13.6497276187075));
#20666=CARTESIAN_POINT('',(-1.,-1.,13.6497276187075));
#20667=CARTESIAN_POINT('',(-1.,-1.,13.7839017669334));
#20668=CARTESIAN_POINT('',(-1.,1.,13.6497276187075));
#20669=CARTESIAN_POINT('',(-1.,1.,13.7839017669334));
#20670=CARTESIAN_POINT('',(-1.,-1.,13.6497276187075));
#20671=CARTESIAN_POINT('Origin',(-1.45,-1.,13.4859410132877));
#20672=CARTESIAN_POINT('',(-1.45,-1.,13.4859410132877));
#20673=CARTESIAN_POINT('',(-1.,-1.,13.6497276187075));
#20674=CARTESIAN_POINT('',(-1.45,1.,13.4859410132877));
#20675=CARTESIAN_POINT('',(-1.,1.,13.6497276187075));
#20676=CARTESIAN_POINT('',(-1.45,-1.,13.4859410132877));
#20677=CARTESIAN_POINT('Origin',(-1.45,-1.,13.3193698416352));
#20678=CARTESIAN_POINT('',(-1.45,-1.,13.3193698416352));
#20679=CARTESIAN_POINT('',(-1.45,-1.,13.4859410132877));
#20680=CARTESIAN_POINT('',(-1.45,1.,13.3193698416352));
#20681=CARTESIAN_POINT('',(-1.45,1.,13.4859410132877));
#20682=CARTESIAN_POINT('',(-1.45,-1.,13.3193698416352));
#20683=CARTESIAN_POINT('Origin',(-1.,-1.,13.1555832362154));
#20684=CARTESIAN_POINT('',(-1.,-1.,13.1555832362154));
#20685=CARTESIAN_POINT('',(-1.45,-1.,13.3193698416352));
#20686=CARTESIAN_POINT('',(-1.,1.,13.1555832362154));
#20687=CARTESIAN_POINT('',(-1.45,1.,13.3193698416352));
#20688=CARTESIAN_POINT('',(-1.,-1.,13.1555832362154));
#20689=CARTESIAN_POINT('Origin',(-1.,-1.,13.0214090879895));
#20690=CARTESIAN_POINT('',(-1.,-1.,13.0214090879895));
#20691=CARTESIAN_POINT('',(-1.,-1.,13.1555832362154));
#20692=CARTESIAN_POINT('',(-1.,1.,13.0214090879895));
#20693=CARTESIAN_POINT('',(-1.,1.,13.1555832362154));
#20694=CARTESIAN_POINT('',(-1.,-1.,13.0214090879895));
#20695=CARTESIAN_POINT('Origin',(-1.45,-1.,12.8576224825697));
#20696=CARTESIAN_POINT('',(-1.45,-1.,12.8576224825697));
#20697=CARTESIAN_POINT('',(-1.,-1.,13.0214090879895));
#20698=CARTESIAN_POINT('',(-1.45,1.,12.8576224825697));
#20699=CARTESIAN_POINT('',(-1.,1.,13.0214090879895));
#20700=CARTESIAN_POINT('',(-1.45,-1.,12.8576224825697));
#20701=CARTESIAN_POINT('Origin',(-1.45,-1.,12.6910513109172));
#20702=CARTESIAN_POINT('',(-1.45,-1.,12.6910513109172));
#20703=CARTESIAN_POINT('',(-1.45,-1.,12.8576224825697));
#20704=CARTESIAN_POINT('',(-1.45,1.,12.6910513109172));
#20705=CARTESIAN_POINT('',(-1.45,1.,12.8576224825697));
#20706=CARTESIAN_POINT('',(-1.45,-1.,12.6910513109172));
#20707=CARTESIAN_POINT('Origin',(-1.,-1.,12.5272647054974));
#20708=CARTESIAN_POINT('',(-1.,-1.,12.5272647054974));
#20709=CARTESIAN_POINT('',(-1.45,-1.,12.6910513109172));
#20710=CARTESIAN_POINT('',(-1.,1.,12.5272647054974));
#20711=CARTESIAN_POINT('',(-1.45,1.,12.6910513109172));
#20712=CARTESIAN_POINT('',(-1.,-1.,12.5272647054974));
#20713=CARTESIAN_POINT('Origin',(-1.,-1.,12.3930905572716));
#20714=CARTESIAN_POINT('',(-1.,-1.,12.3930905572716));
#20715=CARTESIAN_POINT('',(-1.,-1.,12.5272647054974));
#20716=CARTESIAN_POINT('',(-1.,1.,12.3930905572716));
#20717=CARTESIAN_POINT('',(-1.,1.,12.5272647054974));
#20718=CARTESIAN_POINT('',(-1.,-1.,12.3930905572716));
#20719=CARTESIAN_POINT('Origin',(-1.45,-1.,12.2293039518518));
#20720=CARTESIAN_POINT('',(-1.45,-1.,12.2293039518518));
#20721=CARTESIAN_POINT('',(-1.,-1.,12.3930905572716));
#20722=CARTESIAN_POINT('',(-1.45,1.,12.2293039518518));
#20723=CARTESIAN_POINT('',(-1.,1.,12.3930905572716));
#20724=CARTESIAN_POINT('',(-1.45,-1.,12.2293039518518));
#20725=CARTESIAN_POINT('Origin',(-1.45,-1.,12.0627327801993));
#20726=CARTESIAN_POINT('',(-1.45,-1.,12.0627327801993));
#20727=CARTESIAN_POINT('',(-1.45,-1.,12.2293039518518));
#20728=CARTESIAN_POINT('',(-1.45,1.,12.0627327801993));
#20729=CARTESIAN_POINT('',(-1.45,1.,12.2293039518518));
#20730=CARTESIAN_POINT('',(-1.45,-1.,12.0627327801993));
#20731=CARTESIAN_POINT('Origin',(-1.,-1.,11.8989461747795));
#20732=CARTESIAN_POINT('',(-1.,-1.,11.8989461747795));
#20733=CARTESIAN_POINT('',(-1.45,-1.,12.0627327801993));
#20734=CARTESIAN_POINT('',(-1.,1.,11.8989461747795));
#20735=CARTESIAN_POINT('',(-1.45,1.,12.0627327801993));
#20736=CARTESIAN_POINT('',(-1.,-1.,11.8989461747795));
#20737=CARTESIAN_POINT('Origin',(-1.,-1.,11.7647720265536));
#20738=CARTESIAN_POINT('',(-1.,-1.,11.7647720265536));
#20739=CARTESIAN_POINT('',(-1.,-1.,11.8989461747795));
#20740=CARTESIAN_POINT('',(-1.,1.,11.7647720265536));
#20741=CARTESIAN_POINT('',(-1.,1.,11.8989461747795));
#20742=CARTESIAN_POINT('',(-1.,-1.,11.7647720265536));
#20743=CARTESIAN_POINT('Origin',(-1.45,-1.,11.6009854211338));
#20744=CARTESIAN_POINT('',(-1.45,-1.,11.6009854211338));
#20745=CARTESIAN_POINT('',(-1.,-1.,11.7647720265536));
#20746=CARTESIAN_POINT('',(-1.45,1.,11.6009854211338));
#20747=CARTESIAN_POINT('',(-1.,1.,11.7647720265536));
#20748=CARTESIAN_POINT('',(-1.45,-1.,11.6009854211338));
#20749=CARTESIAN_POINT('Origin',(-1.45,-1.,11.4344142494813));
#20750=CARTESIAN_POINT('',(-1.45,-1.,11.4344142494813));
#20751=CARTESIAN_POINT('',(-1.45,-1.,11.6009854211338));
#20752=CARTESIAN_POINT('',(-1.45,1.,11.4344142494813));
#20753=CARTESIAN_POINT('',(-1.45,1.,11.6009854211338));
#20754=CARTESIAN_POINT('',(-1.45,-1.,11.4344142494813));
#20755=CARTESIAN_POINT('Origin',(-1.,-1.,11.2706276440615));
#20756=CARTESIAN_POINT('',(-1.,-1.,11.2706276440615));
#20757=CARTESIAN_POINT('',(-1.45,-1.,11.4344142494813));
#20758=CARTESIAN_POINT('',(-1.,1.,11.2706276440615));
#20759=CARTESIAN_POINT('',(-1.45,1.,11.4344142494813));
#20760=CARTESIAN_POINT('',(-1.,-1.,11.2706276440615));
#20761=CARTESIAN_POINT('Origin',(-1.,-1.,11.));
#20762=CARTESIAN_POINT('',(-1.,-1.,11.2706276440615));
#20763=CARTESIAN_POINT('',(-1.,1.,11.2706276440615));
#20764=CARTESIAN_POINT('Origin',(-0.625,1.,24.));
#20765=CARTESIAN_POINT('Origin',(-0.625,-1.,24.));
#20766=CARTESIAN_POINT('Origin',(1.,0.,10.8));
#20767=CARTESIAN_POINT('',(0.,-1.22464679914735E-16,40.));
#20768=CARTESIAN_POINT('Origin',(1.,0.,40.));
#20769=CARTESIAN_POINT('',(0.,-1.22464679914735E-16,10.8));
#20770=CARTESIAN_POINT('',(0.,-1.22464679914735E-16,10.8));
#20771=CARTESIAN_POINT('',(0.,-1.22464679914735E-16,10.8));
#20772=CARTESIAN_POINT('Origin',(1.,0.,10.8));
#20773=CARTESIAN_POINT('Origin',(1.,0.,40.));
#20774=CARTESIAN_POINT('Origin',(1.,0.,10.8));
#20775=CARTESIAN_POINT('',(0.,0.,0.));
#20776=CARTESIAN_POINT('Origin',(1.29,0.,10.4));
#20777=CARTESIAN_POINT('',(1.29,0.0768114574786861,10.2539691813349));
#20778=CARTESIAN_POINT('',(1.29,0.0768114574786861,10.5460308186651));
#20779=CARTESIAN_POINT('',(1.29,0.0768114574786861,9.9));
#20780=CARTESIAN_POINT('Origin',(1.29,0.,10.4));
#20781=CARTESIAN_POINT('Origin',(1.29,0.,10.4));
#20782=CARTESIAN_POINT('',(1.29,-0.0768114574786861,10.2539691813349));
#20783=CARTESIAN_POINT('Ctrl Pts',(1.29,-0.0768114574786869,10.2539691813349));
#20784=CARTESIAN_POINT('Ctrl Pts',(1.29112130391241,-0.0725779987568773,
10.2517424038809));
#20785=CARTESIAN_POINT('Ctrl Pts',(1.29217403693718,-0.0682275444786245,
10.2496896532208));
#20786=CARTESIAN_POINT('Ctrl Pts',(1.29755094970157,-0.0435167473439239,
10.2393317115009));
#20787=CARTESIAN_POINT('Ctrl Pts',(1.3,-0.0212025739403112,10.235));
#20788=CARTESIAN_POINT('Ctrl Pts',(1.3,0.0212025739403112,10.235));
#20789=CARTESIAN_POINT('Ctrl Pts',(1.29755094970157,0.0435167473439239,
10.2393317115009));
#20790=CARTESIAN_POINT('Ctrl Pts',(1.29217403693718,0.0682275444786249,
10.2496896532208));
#20791=CARTESIAN_POINT('Ctrl Pts',(1.29112130391241,0.0725779987568771,
10.2517424038809));
#20792=CARTESIAN_POINT('Ctrl Pts',(1.29,0.0768114574786869,10.2539691813349));
#20793=CARTESIAN_POINT('',(1.29,-0.0768114574786861,10.5460308186651));
#20794=CARTESIAN_POINT('Origin',(1.29,0.,10.4));
#20795=CARTESIAN_POINT('',(1.3,-6.633889141012E-18,10.565));
#20796=CARTESIAN_POINT('Ctrl Pts',(1.3,3.46944695195361E-17,10.565));
#20797=CARTESIAN_POINT('Ctrl Pts',(1.3,-0.0212025739403111,10.565));
#20798=CARTESIAN_POINT('Ctrl Pts',(1.29755094970157,-0.043516747343924,
10.5606682884991));
#20799=CARTESIAN_POINT('Ctrl Pts',(1.29217403693718,-0.0682275444786246,
10.5503103467792));
#20800=CARTESIAN_POINT('Ctrl Pts',(1.29112130391241,-0.072577998756877,
10.5482575961191));
#20801=CARTESIAN_POINT('Ctrl Pts',(1.29,-0.0768114574786861,10.5460308186651));
#20802=CARTESIAN_POINT('',(2.4,-2.02066721859312E-17,10.565));
#20803=CARTESIAN_POINT('',(1.29,-2.02066721859312E-17,10.565));
#20804=CARTESIAN_POINT('',(2.3902427845524,0.164999999999999,10.4));
#20805=CARTESIAN_POINT('Ctrl Pts',(2.3902427845524,0.164999999999999,10.4));
#20806=CARTESIAN_POINT('Ctrl Pts',(2.3902427845524,0.164999999999999,10.37926146026));
#20807=CARTESIAN_POINT('Ctrl Pts',(2.39075468722975,0.160851447474558,10.3571538860416));
#20808=CARTESIAN_POINT('Ctrl Pts',(2.39259968365095,0.144006627864299,10.3165070705051));
#20809=CARTESIAN_POINT('Ctrl Pts',(2.39390570229761,0.131311408395221,10.2979661706037));
#20810=CARTESIAN_POINT('Ctrl Pts',(2.39635413416378,0.102033925885227,10.2686886880937));
#20811=CARTESIAN_POINT('Ctrl Pts',(2.39765618378145,0.0834929839417275,
10.2559933930893));
#20812=CARTESIAN_POINT('Ctrl Pts',(2.39949208802221,0.042846026446056,10.2391485178689));
#20813=CARTESIAN_POINT('Ctrl Pts',(2.4,0.0207384030457212,10.235));
#20814=CARTESIAN_POINT('Ctrl Pts',(2.4,-0.0207384030457212,10.235));
#20815=CARTESIAN_POINT('Ctrl Pts',(2.39949208802221,-0.042846026446056,
10.2391485178689));
#20816=CARTESIAN_POINT('Ctrl Pts',(2.39765618378145,-0.0834929839417275,
10.2559933930893));
#20817=CARTESIAN_POINT('Ctrl Pts',(2.39635413416378,-0.102033925885227,
10.2686886880937));
#20818=CARTESIAN_POINT('Ctrl Pts',(2.39390570229761,-0.131311408395221,
10.2979661706037));
#20819=CARTESIAN_POINT('Ctrl Pts',(2.39259968365095,-0.144006627864299,
10.3165070705051));
#20820=CARTESIAN_POINT('Ctrl Pts',(2.39075468722975,-0.160851447474558,
10.3571538860416));
#20821=CARTESIAN_POINT('Ctrl Pts',(2.3902427845524,-0.164999999999999,10.37926146026));
#20822=CARTESIAN_POINT('Ctrl Pts',(2.3902427845524,-0.164999999999999,10.42073853974));
#20823=CARTESIAN_POINT('Ctrl Pts',(2.39075468722975,-0.160851447474558,
10.4428461139584));
#20824=CARTESIAN_POINT('Ctrl Pts',(2.39259968365095,-0.144006627864299,
10.4834929294949));
#20825=CARTESIAN_POINT('Ctrl Pts',(2.39390570229761,-0.131311408395221,
10.5020338293963));
#20826=CARTESIAN_POINT('Ctrl Pts',(2.39635413416378,-0.102033925885227,
10.5313113119063));
#20827=CARTESIAN_POINT('Ctrl Pts',(2.39765618378145,-0.0834929839417275,
10.5440066069107));
#20828=CARTESIAN_POINT('Ctrl Pts',(2.39949208802221,-0.042846026446056,
10.5608514821311));
#20829=CARTESIAN_POINT('Ctrl Pts',(2.4,-0.0207384030457212,10.565));
#20830=CARTESIAN_POINT('Ctrl Pts',(2.4,-2.60208521396521E-17,10.565));
#20831=CARTESIAN_POINT('Ctrl Pts',(2.4,1.04083408558608E-16,10.565));
#20832=CARTESIAN_POINT('Ctrl Pts',(2.4,0.0207384030457213,10.565));
#20833=CARTESIAN_POINT('Ctrl Pts',(2.39949208802221,0.042846026446056,10.5608514821311));
#20834=CARTESIAN_POINT('Ctrl Pts',(2.39765618378145,0.0834929839417275,
10.5440066069107));
#20835=CARTESIAN_POINT('Ctrl Pts',(2.39635413416378,0.102033925885227,10.5313113119063));
#20836=CARTESIAN_POINT('Ctrl Pts',(2.39390570229761,0.131311408395221,10.5020338293963));
#20837=CARTESIAN_POINT('Ctrl Pts',(2.39259968365095,0.144006627864299,10.4834929294949));
#20838=CARTESIAN_POINT('Ctrl Pts',(2.39075468722975,0.160851447474558,10.4428461139584));
#20839=CARTESIAN_POINT('Ctrl Pts',(2.3902427845524,0.164999999999999,10.42073853974));
#20840=CARTESIAN_POINT('Ctrl Pts',(2.3902427845524,0.164999999999999,10.4));
#20841=CARTESIAN_POINT('Ctrl Pts',(1.29,0.0768114574786861,10.5460308186651));
#20842=CARTESIAN_POINT('Ctrl Pts',(1.29112130391241,0.0725779987568767,
10.5482575961191));
#20843=CARTESIAN_POINT('Ctrl Pts',(1.29217403693718,0.0682275444786243,
10.5503103467792));
#20844=CARTESIAN_POINT('Ctrl Pts',(1.29755094970157,0.0435167473439239,
10.5606682884991));
#20845=CARTESIAN_POINT('Ctrl Pts',(1.3,0.0212025739403111,10.565));
#20846=CARTESIAN_POINT('Ctrl Pts',(1.3,-4.16333634234434E-17,10.565));
#20847=CARTESIAN_POINT('Origin',(1.29,0.,10.4));
#20848=CARTESIAN_POINT('',(1.29,-0.0768114574786861,9.9));
#20849=CARTESIAN_POINT('Origin',(1.,0.,9.9));
#20850=CARTESIAN_POINT('',(0.7,-3.67394039744206E-17,10.));
#20851=CARTESIAN_POINT('Origin',(1.,0.,10.));
#20852=CARTESIAN_POINT('',(0.7,3.67394039744206E-17,11.8));
#20853=CARTESIAN_POINT('',(0.7,-3.67394039744206E-17,9.9));
#20854=CARTESIAN_POINT('Origin',(1.,0.,11.8));
#20855=CARTESIAN_POINT('Origin',(1.,0.,10.8));
#20856=CARTESIAN_POINT('',(0.5,-6.12323399573677E-17,11.8));
#20857=CARTESIAN_POINT('Origin',(1.,0.,11.8));
#20858=CARTESIAN_POINT('',(0.5,-6.12323399573677E-17,10.8));
#20859=CARTESIAN_POINT('',(0.5,-6.12323399573677E-17,10.8));
#20860=CARTESIAN_POINT('Origin',(1.,0.,10.8));
#20861=CARTESIAN_POINT('Origin',(1.,0.,11.8));
#20862=CARTESIAN_POINT('Origin',(1.,0.,10.));
#20863=CARTESIAN_POINT('',(-0.4,-1.71450551880629E-16,10.8));
#20864=CARTESIAN_POINT('Origin',(1.,0.,10.8));
#20865=CARTESIAN_POINT('',(-0.4,-1.71450551880629E-16,10.));
#20866=CARTESIAN_POINT('',(-0.4,-1.71450551880629E-16,10.));
#20867=CARTESIAN_POINT('Origin',(1.,0.,10.));
#20868=CARTESIAN_POINT('Origin',(1.,0.,10.8));
#20869=CARTESIAN_POINT('Origin',(1.,0.,10.));
#20870=CARTESIAN_POINT('',(0.,0.,0.));
#20871=CARTESIAN_POINT('Origin',(1.,0.,7.));
#20872=CARTESIAN_POINT('',(0.7,-3.67394039744206E-17,10.5));
#20873=CARTESIAN_POINT('Origin',(1.,0.,10.5));
#20874=CARTESIAN_POINT('',(0.7,-3.67394039744206E-17,7.));
#20875=CARTESIAN_POINT('',(0.7,-3.67394039744206E-17,7.));
#20876=CARTESIAN_POINT('Origin',(1.,0.,7.));
#20877=CARTESIAN_POINT('Origin',(1.,0.,10.5));
#20878=CARTESIAN_POINT('Origin',(1.,0.,7.));
#20879=CARTESIAN_POINT('',(0.,0.,0.));
#20880=CARTESIAN_POINT('Origin',(1.3,0.,10.4));
#20881=CARTESIAN_POINT('',(2.4,-2.4492935982947E-17,10.6));
#20882=CARTESIAN_POINT('Origin',(2.4,0.,10.4));
#20883=CARTESIAN_POINT('',(1.3,-2.4492935982947E-17,10.6));
#20884=CARTESIAN_POINT('',(1.3,-2.4492935982947E-17,10.6));
#20885=CARTESIAN_POINT('Origin',(1.3,0.,10.4));
#20886=CARTESIAN_POINT('Origin',(2.4,0.,10.4));
#20887=CARTESIAN_POINT('Origin',(1.3,0.,10.4));
#20888=CARTESIAN_POINT('',(0.,0.,0.));
#20889=CARTESIAN_POINT('Origin',(1.99,0.,30.));
#20890=CARTESIAN_POINT('',(1.9913626985115,0.164999999999999,30.));
#20891=CARTESIAN_POINT('',(2.005,-8.29617220839915E-17,30.165));
#20892=CARTESIAN_POINT('Ctrl Pts',(1.9913626985115,0.164999999999999,30.));
#20893=CARTESIAN_POINT('Ctrl Pts',(1.9913626985115,0.164999999999999,30.0207584616532));
#20894=CARTESIAN_POINT('Ctrl Pts',(1.99208213234536,0.160843707720236,30.0428743626922));
#20895=CARTESIAN_POINT('Ctrl Pts',(1.99466757507705,0.143993298000808,30.0835155100945));
#20896=CARTESIAN_POINT('Ctrl Pts',(1.9964948147884,0.131301190829395,30.1020440469622));
#20897=CARTESIAN_POINT('Ctrl Pts',(1.99991441892026,0.102044414577984,30.1313008232136));
#20898=CARTESIAN_POINT('Ctrl Pts',(2.00173085232892,0.0835157197655822,
30.1439932187437));
#20899=CARTESIAN_POINT('Ctrl Pts',(2.00429148829838,0.0428740302308141,
30.1608438378879));
#20900=CARTESIAN_POINT('Ctrl Pts',(2.005,0.0207579399932888,30.165));
#20901=CARTESIAN_POINT('Ctrl Pts',(2.005,2.35922392732846E-16,30.165));
#20902=CARTESIAN_POINT('Ctrl Pts',(2.005,-1.52655665885959E-16,30.165));
#20903=CARTESIAN_POINT('Ctrl Pts',(2.005,-0.0207579399932887,30.165));
#20904=CARTESIAN_POINT('Ctrl Pts',(2.00429148829838,-0.0428740302308141,
30.1608438378879));
#20905=CARTESIAN_POINT('Ctrl Pts',(2.00173085232892,-0.0835157197655809,
30.1439932187437));
#20906=CARTESIAN_POINT('Ctrl Pts',(1.99991441892026,-0.102044414577984,
30.1313008232136));
#20907=CARTESIAN_POINT('Ctrl Pts',(1.9964948147884,-0.131301190829395,30.1020440469622));
#20908=CARTESIAN_POINT('Ctrl Pts',(1.99466757507705,-0.143993298000808,
30.0835155100945));
#20909=CARTESIAN_POINT('Ctrl Pts',(1.99208213234536,-0.160843707720236,
30.0428743626922));
#20910=CARTESIAN_POINT('Ctrl Pts',(1.9913626985115,-0.164999999999999,30.0207584616532));
#20911=CARTESIAN_POINT('Ctrl Pts',(1.9913626985115,-0.164999999999999,29.9792415383468));
#20912=CARTESIAN_POINT('Ctrl Pts',(1.99208213234536,-0.160843707720236,
29.9571256373078));
#20913=CARTESIAN_POINT('Ctrl Pts',(1.99466757507705,-0.143993298000808,
29.9164844899055));
#20914=CARTESIAN_POINT('Ctrl Pts',(1.9964948147884,-0.131301190829395,29.8979559530378));
#20915=CARTESIAN_POINT('Ctrl Pts',(1.99991441892026,-0.102044414577984,
29.8686991767864));
#20916=CARTESIAN_POINT('Ctrl Pts',(2.00173085232892,-0.0835157197655809,
29.8560067812563));
#20917=CARTESIAN_POINT('Ctrl Pts',(2.00429148829838,-0.0428740302308141,
29.8391561621121));
#20918=CARTESIAN_POINT('Ctrl Pts',(2.005,-0.0207579399932886,29.835));
#20919=CARTESIAN_POINT('Ctrl Pts',(2.005,0.0207579399932885,29.835));
#20920=CARTESIAN_POINT('Ctrl Pts',(2.00429148829838,0.042874030230814,29.8391561621121));
#20921=CARTESIAN_POINT('Ctrl Pts',(2.00173085232892,0.0835157197655809,
29.8560067812563));
#20922=CARTESIAN_POINT('Ctrl Pts',(1.99991441892026,0.102044414577984,29.8686991767864));
#20923=CARTESIAN_POINT('Ctrl Pts',(1.9964948147884,0.131301190829395,29.8979559530378));
#20924=CARTESIAN_POINT('Ctrl Pts',(1.99466757507705,0.143993298000808,29.9164844899055));
#20925=CARTESIAN_POINT('Ctrl Pts',(1.99208213234536,0.160843707720236,29.9571256373078));
#20926=CARTESIAN_POINT('Ctrl Pts',(1.9913626985115,0.164999999999999,29.9792415383468));
#20927=CARTESIAN_POINT('Ctrl Pts',(1.9913626985115,0.164999999999999,30.));
#20928=CARTESIAN_POINT('',(2.7,-2.02066721859312E-17,30.165));
#20929=CARTESIAN_POINT('',(1.99,-2.02066721859312E-17,30.165));
#20930=CARTESIAN_POINT('',(2.69197369955919,0.164999999999999,30.));
#20931=CARTESIAN_POINT('Ctrl Pts',(2.69197369955919,0.164999999999999,30.));
#20932=CARTESIAN_POINT('Ctrl Pts',(2.69197369955919,0.164999999999999,29.9792681899326));
#20933=CARTESIAN_POINT('Ctrl Pts',(2.69239400387291,0.160854068850877,29.9571634685398));
#20934=CARTESIAN_POINT('Ctrl Pts',(2.69391035162893,0.14401116680132,29.9165147673388));
#20935=CARTESIAN_POINT('Ctrl Pts',(2.69498430847444,0.13131490896209,29.8979696711705));
#20936=CARTESIAN_POINT('Ctrl Pts',(2.69699888419766,0.102030373034454,29.8686851352429));
#20937=CARTESIAN_POINT('Ctrl Pts',(2.69807062966546,0.0834852574625918,
29.8559888429375));
#20938=CARTESIAN_POINT('Ctrl Pts',(2.69958191522061,0.0428364913743715,
29.8391459150772));
#20939=CARTESIAN_POINT('Ctrl Pts',(2.7,0.0207317474782039,29.835));
#20940=CARTESIAN_POINT('Ctrl Pts',(2.7,-0.0207317474782039,29.835));
#20941=CARTESIAN_POINT('Ctrl Pts',(2.69958191522061,-0.0428364913743715,
29.8391459150772));
#20942=CARTESIAN_POINT('Ctrl Pts',(2.69807062966546,-0.0834852574625918,
29.8559888429375));
#20943=CARTESIAN_POINT('Ctrl Pts',(2.69699888419766,-0.102030373034454,
29.8686851352429));
#20944=CARTESIAN_POINT('Ctrl Pts',(2.69498430847444,-0.13131490896209,29.8979696711705));
#20945=CARTESIAN_POINT('Ctrl Pts',(2.69391035162893,-0.14401116680132,29.9165147673388));
#20946=CARTESIAN_POINT('Ctrl Pts',(2.69239400387291,-0.160854068850877,
29.9571634685398));
#20947=CARTESIAN_POINT('Ctrl Pts',(2.69197369955919,-0.164999999999999,
29.9792681899326));
#20948=CARTESIAN_POINT('Ctrl Pts',(2.69197369955919,-0.164999999999999,
30.0207318100674));
#20949=CARTESIAN_POINT('Ctrl Pts',(2.69239400387291,-0.160854068850877,
30.0428365314602));
#20950=CARTESIAN_POINT('Ctrl Pts',(2.69391035162893,-0.14401116680132,30.0834852326612));
#20951=CARTESIAN_POINT('Ctrl Pts',(2.69498430847444,-0.13131490896209,30.1020303288295));
#20952=CARTESIAN_POINT('Ctrl Pts',(2.69699888419766,-0.102030373034454,
30.1313148647571));
#20953=CARTESIAN_POINT('Ctrl Pts',(2.69807062966546,-0.0834852574625918,
30.1440111570625));
#20954=CARTESIAN_POINT('Ctrl Pts',(2.69958191522061,-0.0428364913743716,
30.1608540849228));
#20955=CARTESIAN_POINT('Ctrl Pts',(2.7,-0.0207317474782039,30.165));
#20956=CARTESIAN_POINT('Ctrl Pts',(2.7,6.24500451351651E-17,30.165));
#20957=CARTESIAN_POINT('Ctrl Pts',(2.7,-1.11022302462516E-16,30.165));
#20958=CARTESIAN_POINT('Ctrl Pts',(2.7,0.0207317474782038,30.165));
#20959=CARTESIAN_POINT('Ctrl Pts',(2.69958191522061,0.0428364913743715,
30.1608540849228));
#20960=CARTESIAN_POINT('Ctrl Pts',(2.69807062966546,0.0834852574625918,
30.1440111570625));
#20961=CARTESIAN_POINT('Ctrl Pts',(2.69699888419766,0.102030373034454,30.1313148647571));
#20962=CARTESIAN_POINT('Ctrl Pts',(2.69498430847444,0.13131490896209,30.1020303288295));
#20963=CARTESIAN_POINT('Ctrl Pts',(2.69391035162893,0.14401116680132,30.0834852326612));
#20964=CARTESIAN_POINT('Ctrl Pts',(2.69239400387291,0.160854068850877,30.0428365314602));
#20965=CARTESIAN_POINT('Ctrl Pts',(2.69197369955919,0.164999999999999,30.0207318100674));
#20966=CARTESIAN_POINT('Ctrl Pts',(2.69197369955919,0.164999999999999,30.));
#20967=CARTESIAN_POINT('Origin',(0.21,1.01,29.5));
#20968=CARTESIAN_POINT('',(0.21,1.01,29.6));
#20969=CARTESIAN_POINT('',(-0.367442869007697,1.01,29.6));
#20970=CARTESIAN_POINT('',(0.605,1.01,29.6));
#20971=CARTESIAN_POINT('',(0.21,1.01,30.4));
#20972=CARTESIAN_POINT('',(0.21,1.01,29.5));
#20973=CARTESIAN_POINT('',(-0.367442869007697,1.01,30.4));
#20974=CARTESIAN_POINT('',(0.605,1.01,30.4));
#20975=CARTESIAN_POINT('',(-0.367442869007697,1.01,29.6));
#20976=CARTESIAN_POINT('Origin',(0.21,-1.01,29.5));
#20977=CARTESIAN_POINT('',(0.21,-1.01,29.6));
#20978=CARTESIAN_POINT('',(0.21,-0.621228621362538,29.6));
#20979=CARTESIAN_POINT('',(0.21,-0.505,29.6));
#20980=CARTESIAN_POINT('',(0.21,-1.01,30.4));
#20981=CARTESIAN_POINT('',(0.21,-1.01,29.5));
#20982=CARTESIAN_POINT('',(0.21,-0.621228621362538,30.4));
#20983=CARTESIAN_POINT('',(0.21,-0.505,30.4));
#20984=CARTESIAN_POINT('',(0.21,-0.621228621362538,29.6));
#20985=CARTESIAN_POINT('Origin',(0.21,-1.01,29.5));
#20986=CARTESIAN_POINT('',(0.21,0.621228621362538,29.6));
#20987=CARTESIAN_POINT('',(0.21,-0.505,29.6));
#20988=CARTESIAN_POINT('',(0.21,0.621228621362538,30.4));
#20989=CARTESIAN_POINT('',(0.21,0.621228621362538,29.6));
#20990=CARTESIAN_POINT('',(0.21,-0.505,30.4));
#20991=CARTESIAN_POINT('Origin',(-0.8,-1.01,29.5));
#20992=CARTESIAN_POINT('',(-0.367442869007697,-1.01,29.6));
#20993=CARTESIAN_POINT('',(0.1,-1.01,29.6));
#20994=CARTESIAN_POINT('',(-0.367442869007697,-1.01,30.4));
#20995=CARTESIAN_POINT('',(-0.367442869007697,-1.01,29.6));
#20996=CARTESIAN_POINT('',(0.1,-1.01,30.4));
#20997=CARTESIAN_POINT('Origin',(1.,0.,30.4));
#20998=CARTESIAN_POINT('Origin',(1.,0.,30.4));
#20999=CARTESIAN_POINT('Origin',(1.,0.,30.4));
#21000=CARTESIAN_POINT('Origin',(1.,0.,29.6));
#21001=CARTESIAN_POINT('Origin',(1.,0.,29.6));
#21002=CARTESIAN_POINT('Origin',(1.,0.,29.6));
#21003=CARTESIAN_POINT('Origin',(1.,0.,29.6));
#21004=CARTESIAN_POINT('Origin',(1.,0.,29.6));
#21005=CARTESIAN_POINT('',(0.,0.,0.));
#21006=CARTESIAN_POINT('Origin',(0.0577350269189626,0.,-0.1));
#21007=CARTESIAN_POINT('',(0.0577350269189626,0.,-0.1));
#21008=CARTESIAN_POINT('',(0.115470053837925,0.,0.));
#21009=CARTESIAN_POINT('',(0.0934187836487032,0.,-0.0381939203391614));
#21010=CARTESIAN_POINT('',(0.0577350269189626,-0.2,-0.1));
#21011=CARTESIAN_POINT('',(0.0577350269189626,0.,-0.1));
#21012=CARTESIAN_POINT('',(0.115470053837925,-0.2,0.));
#21013=CARTESIAN_POINT('',(0.115470053837925,-0.2,0.));
#21014=CARTESIAN_POINT('',(0.115470053837925,0.,0.));
#21015=CARTESIAN_POINT('Origin',(-0.0577350269189626,0.,-0.1));
#21016=CARTESIAN_POINT('',(-0.0577350269189626,0.,-0.1));
#21017=CARTESIAN_POINT('',(0.0561324865405187,0.,-0.1));
#21018=CARTESIAN_POINT('',(-0.0577350269189626,-0.2,-0.1));
#21019=CARTESIAN_POINT('',(-0.0577350269189626,0.,-0.1));
#21020=CARTESIAN_POINT('',(0.0577350269189626,-0.2,-0.1));
#21021=CARTESIAN_POINT('Origin',(-0.115470053837925,0.,-1.38777878078145E-17));
#21022=CARTESIAN_POINT('',(-0.115470053837925,0.,-1.41410031829988E-17));
#21023=CARTESIAN_POINT('',(-0.0797862971081845,0.,-0.0618060796608387));
#21024=CARTESIAN_POINT('',(-0.115470053837925,-0.2,-1.38777878078145E-17));
#21025=CARTESIAN_POINT('',(-0.115470053837925,0.,-1.41410031829988E-17));
#21026=CARTESIAN_POINT('',(-0.0577350269189626,-0.2,-0.1));
#21027=CARTESIAN_POINT('Origin',(-0.0577350269189626,0.,0.1));
#21028=CARTESIAN_POINT('',(-0.0577350269189626,0.,0.1));
#21029=CARTESIAN_POINT('',(-0.0509187836487033,0.,0.111806079660839));
#21030=CARTESIAN_POINT('',(-0.0577350269189626,-0.2,0.1));
#21031=CARTESIAN_POINT('',(-0.0577350269189626,0.,0.1));
#21032=CARTESIAN_POINT('',(-0.115470053837925,-0.2,-1.41410031829988E-17));
#21033=CARTESIAN_POINT('Origin',(0.0577350269189626,0.,0.1));
#21034=CARTESIAN_POINT('',(0.0577350269189626,0.,0.1));
#21035=CARTESIAN_POINT('',(0.113867513459481,0.,0.1));
#21036=CARTESIAN_POINT('',(0.0577350269189626,-0.2,0.1));
#21037=CARTESIAN_POINT('',(0.0577350269189626,0.,0.1));
#21038=CARTESIAN_POINT('',(-0.0577350269189626,-0.2,0.1));
#21039=CARTESIAN_POINT('Origin',(0.115470053837925,0.,0.));
#21040=CARTESIAN_POINT('',(0.122286297108185,0.,-0.0118060796608386));
#21041=CARTESIAN_POINT('',(0.0577350269189626,-0.2,0.1));
#21042=CARTESIAN_POINT('Origin',(0.,-0.2,0.));
#21043=CARTESIAN_POINT('Origin',(0.17,0.,0.));
#21044=CARTESIAN_POINT('',(-0.17,-8.67361737988404E-18,-2.0818995585505E-17));
#21045=CARTESIAN_POINT('Origin',(0.,0.,0.));
#21046=CARTESIAN_POINT('Origin',(0.,-0.015,0.));
#21047=CARTESIAN_POINT('',(-0.1954,-0.0254,-2.39295984553393E-17));
#21048=CARTESIAN_POINT('Origin',(0.,-0.0254,0.));
#21049=CARTESIAN_POINT('',(-0.185,-0.015,-2.2655965784226E-17));
#21050=CARTESIAN_POINT('Origin',(0.,-0.2775,0.));
#21051=CARTESIAN_POINT('',(-0.1954,-0.5296,2.39295984553393E-17));
#21052=CARTESIAN_POINT('Origin',(0.,-0.5296,0.));
#21053=CARTESIAN_POINT('',(-0.1954,-0.2775,-2.39295984553393E-17));
#21054=CARTESIAN_POINT('Origin',(0.,-0.5625,0.));
#21055=CARTESIAN_POINT('',(-0.125,-0.6,-1.53080849893419E-17));
#21056=CARTESIAN_POINT('Origin',(0.,-0.6,0.));
#21057=CARTESIAN_POINT('',(-0.1625,-0.5625,-1.99005104861445E-17));
#21058=CARTESIAN_POINT('Origin',(0.,-0.6,0.));
#21059=CARTESIAN_POINT('',(0.,0.,0.));
#21060=CARTESIAN_POINT('',(0.,0.,0.));
#21061=CARTESIAN_POINT('',(0.,0.,0.));
#21062=CARTESIAN_POINT('',(0.,0.,0.));
#21063=CARTESIAN_POINT('',(0.,0.,0.));
#21064=CARTESIAN_POINT('',(2.6,0.,30.));
#21065=CARTESIAN_POINT('',(0.,0.,0.));
#21066=CARTESIAN_POINT('',(0.,0.,0.));
#21067=CARTESIAN_POINT('Origin',(-3.25,6.,20.));
#21068=CARTESIAN_POINT('',(-3.415,6.,20.));
#21069=CARTESIAN_POINT('Origin',(-3.25,6.,20.));
#21070=CARTESIAN_POINT('',(-3.415,7.5,20.));
#21071=CARTESIAN_POINT('',(-3.415,6.,20.));
#21072=CARTESIAN_POINT('Origin',(-3.25,7.5,20.));
#21073=CARTESIAN_POINT('Origin',(-3.25,6.,20.));
#21074=CARTESIAN_POINT('Origin',(-3.25,-5.6,20.));
#21075=CARTESIAN_POINT('',(-3.415,-5.5,20.));
#21076=CARTESIAN_POINT('Origin',(-3.25,-5.5,20.));
#21077=CARTESIAN_POINT('',(-3.415,-3.9,20.));
#21078=CARTESIAN_POINT('',(-3.415,-5.6,20.));
#21079=CARTESIAN_POINT('Origin',(-3.25,-3.9,20.));
#21080=CARTESIAN_POINT('Origin',(-3.25,-3.9,20.));
#21081=CARTESIAN_POINT('Origin',(-2.55,5.5,19.8));
#21082=CARTESIAN_POINT('',(-2.68431457505076,6.9,19.8));
#21083=CARTESIAN_POINT('',(-2.68431457505076,5.5,19.8));
#21084=CARTESIAN_POINT('',(-2.68431457505076,-5.5,19.8));
#21085=CARTESIAN_POINT('',(-2.9,6.9,19.8));
#21086=CARTESIAN_POINT('',(-2.9,6.9,19.8));
#21087=CARTESIAN_POINT('',(-2.9,5.5,19.8));
#21088=CARTESIAN_POINT('',(-2.9,5.5,19.8));
#21089=CARTESIAN_POINT('',(-2.9,5.5,19.8));
#21090=CARTESIAN_POINT('Origin',(-2.725,5.5,20.));
#21091=CARTESIAN_POINT('',(-2.68431457505076,5.5,20.2));
#21092=CARTESIAN_POINT('Origin',(-3.25,5.5,20.));
#21093=CARTESIAN_POINT('',(-2.9,5.5,20.2));
#21094=CARTESIAN_POINT('',(-2.9,5.5,20.2));
#21095=CARTESIAN_POINT('',(-2.55,5.5,20.2));
#21096=CARTESIAN_POINT('Origin',(-2.9,5.5,19.8));
#21097=CARTESIAN_POINT('',(-2.9,6.9,20.2));
#21098=CARTESIAN_POINT('',(-2.9,6.9,20.2));
#21099=CARTESIAN_POINT('',(-2.9,5.5,20.2));
#21100=CARTESIAN_POINT('Origin',(-2.9,5.5,20.2));
#21101=CARTESIAN_POINT('',(-2.68431457505076,6.9,20.2));
#21102=CARTESIAN_POINT('',(-2.68431457505076,-5.5,20.2));
#21103=CARTESIAN_POINT('',(-2.55,6.9,20.2));
#21104=CARTESIAN_POINT('Origin',(-2.725,6.9,20.));
#21105=CARTESIAN_POINT('Origin',(-3.25,6.9,20.));
#21106=CARTESIAN_POINT('Origin',(-2.55,-0.2,19.8));
#21107=CARTESIAN_POINT('',(-2.68431457505076,1.2,19.8));
#21108=CARTESIAN_POINT('',(-2.68431457505076,-0.2,19.8));
#21109=CARTESIAN_POINT('',(-2.68431457505076,-5.5,19.8));
#21110=CARTESIAN_POINT('',(-2.9,1.2,19.8));
#21111=CARTESIAN_POINT('',(-2.9,1.2,19.8));
#21112=CARTESIAN_POINT('',(-2.9,-0.2,19.8));
#21113=CARTESIAN_POINT('',(-2.9,-0.2,19.8));
#21114=CARTESIAN_POINT('',(-2.9,-0.2,19.8));
#21115=CARTESIAN_POINT('Origin',(-2.725,-0.2,20.));
#21116=CARTESIAN_POINT('',(-2.68431457505076,-0.2,20.2));
#21117=CARTESIAN_POINT('Origin',(-3.25,-0.2,20.));
#21118=CARTESIAN_POINT('',(-2.9,-0.2,20.2));
#21119=CARTESIAN_POINT('',(-2.9,-0.2,20.2));
#21120=CARTESIAN_POINT('',(-2.55,-0.2,20.2));
#21121=CARTESIAN_POINT('Origin',(-2.9,-0.2,19.8));
#21122=CARTESIAN_POINT('',(-2.9,1.2,20.2));
#21123=CARTESIAN_POINT('',(-2.9,1.2,20.2));
#21124=CARTESIAN_POINT('',(-2.9,-0.2,20.2));
#21125=CARTESIAN_POINT('Origin',(-2.9,-0.2,20.2));
#21126=CARTESIAN_POINT('',(-2.68431457505076,1.2,20.2));
#21127=CARTESIAN_POINT('',(-2.68431457505076,-5.5,20.2));
#21128=CARTESIAN_POINT('',(-2.55,1.2,20.2));
#21129=CARTESIAN_POINT('Origin',(-2.725,1.2,20.));
#21130=CARTESIAN_POINT('Origin',(-3.25,1.2,20.));
#21131=CARTESIAN_POINT('Origin',(-3.25,-5.5,20.));
#21132=CARTESIAN_POINT('',(-3.85,7.5,20.));
#21133=CARTESIAN_POINT('Origin',(-3.25,7.5,20.));
#21134=CARTESIAN_POINT('',(-3.85,-5.5,20.));
#21135=CARTESIAN_POINT('',(-3.85,-5.5,20.));
#21136=CARTESIAN_POINT('Origin',(-3.25,-5.5,20.));
#21137=CARTESIAN_POINT('Origin',(-3.25,7.5,20.));
#21138=CARTESIAN_POINT('Origin',(-3.25,-5.5,20.));
#21139=CARTESIAN_POINT('',(0.,0.,0.));
#21140=CARTESIAN_POINT('Origin',(-3.25,-5.5,20.));
#21141=CARTESIAN_POINT('',(-3.855,-3.5,20.));
#21142=CARTESIAN_POINT('Origin',(-3.25,-3.5,20.));
#21143=CARTESIAN_POINT('',(-3.855,-5.5,20.));
#21144=CARTESIAN_POINT('',(-3.855,-5.5,20.));
#21145=CARTESIAN_POINT('Origin',(-3.25,-5.5,20.));
#21146=CARTESIAN_POINT('Origin',(-3.25,-5.5,20.));
#21147=CARTESIAN_POINT('',(-4.05,-3.5,20.));
#21148=CARTESIAN_POINT('Origin',(-3.25,-3.5,20.));
#21149=CARTESIAN_POINT('',(-4.05,-5.5,20.));
#21150=CARTESIAN_POINT('',(-4.05,-5.5,20.));
#21151=CARTESIAN_POINT('Origin',(-3.25,-5.5,20.));
#21152=CARTESIAN_POINT('Origin',(-3.25,-3.5,20.));
#21153=CARTESIAN_POINT('Origin',(-3.25,-5.5,20.));
#21154=CARTESIAN_POINT('',(0.,0.,0.));
#21155=CARTESIAN_POINT('Origin',(-3.25,-2.5,20.));
#21156=CARTESIAN_POINT('',(-3.855,-1.,20.));
#21157=CARTESIAN_POINT('Origin',(-3.25,-1.,20.));
#21158=CARTESIAN_POINT('',(-3.855,-2.5,20.));
#21159=CARTESIAN_POINT('',(-3.855,-2.5,20.));
#21160=CARTESIAN_POINT('Origin',(-3.25,-2.5,20.));
#21161=CARTESIAN_POINT('Origin',(-3.25,-2.5,20.));
#21162=CARTESIAN_POINT('',(-4.05,-1.,20.));
#21163=CARTESIAN_POINT('Origin',(-3.25,-1.,20.));
#21164=CARTESIAN_POINT('',(-4.05,-2.5,20.));
#21165=CARTESIAN_POINT('',(-4.05,-2.5,20.));
#21166=CARTESIAN_POINT('Origin',(-3.25,-2.5,20.));
#21167=CARTESIAN_POINT('Origin',(-3.25,-1.,20.));
#21168=CARTESIAN_POINT('Origin',(-3.25,-2.5,20.));
#21169=CARTESIAN_POINT('',(0.,0.,0.));
#21170=CARTESIAN_POINT('Origin',(-3.25,2.2,20.));
#21171=CARTESIAN_POINT('',(-3.855,2.5,20.));
#21172=CARTESIAN_POINT('Origin',(-3.25,2.5,20.));
#21173=CARTESIAN_POINT('',(-3.855,2.2,20.));
#21174=CARTESIAN_POINT('',(-3.855,2.2,20.));
#21175=CARTESIAN_POINT('Origin',(-3.25,2.2,20.));
#21176=CARTESIAN_POINT('Origin',(-3.25,2.2,20.));
#21177=CARTESIAN_POINT('',(-4.05,2.5,20.));
#21178=CARTESIAN_POINT('Origin',(-3.25,2.5,20.));
#21179=CARTESIAN_POINT('',(-4.05,2.2,20.));
#21180=CARTESIAN_POINT('',(-4.05,2.2,20.));
#21181=CARTESIAN_POINT('Origin',(-3.25,2.2,20.));
#21182=CARTESIAN_POINT('Origin',(-3.25,2.5,20.));
#21183=CARTESIAN_POINT('Origin',(-3.25,2.2,20.));
#21184=CARTESIAN_POINT('',(0.,0.,0.));
#21185=CARTESIAN_POINT('Origin',(-3.25,3.5,20.));
#21186=CARTESIAN_POINT('',(-3.855,5.,20.));
#21187=CARTESIAN_POINT('Origin',(-3.25,5.,20.));
#21188=CARTESIAN_POINT('',(-3.855,3.5,20.));
#21189=CARTESIAN_POINT('',(-3.855,3.5,20.));
#21190=CARTESIAN_POINT('Origin',(-3.25,3.5,20.));
#21191=CARTESIAN_POINT('Origin',(-3.25,3.5,20.));
#21192=CARTESIAN_POINT('',(-4.05,5.,20.));
#21193=CARTESIAN_POINT('Origin',(-3.25,5.,20.));
#21194=CARTESIAN_POINT('',(-4.05,3.5,20.));
#21195=CARTESIAN_POINT('',(-4.05,3.5,20.));
#21196=CARTESIAN_POINT('Origin',(-3.25,3.5,20.));
#21197=CARTESIAN_POINT('Origin',(-3.25,5.,20.));
#21198=CARTESIAN_POINT('Origin',(-3.25,3.5,20.));
#21199=CARTESIAN_POINT('',(0.,0.,0.));
#21200=CARTESIAN_POINT('Origin',(-2.5,1.2,19.8));
#21201=CARTESIAN_POINT('',(-2.5,1.2,19.8));
#21202=CARTESIAN_POINT('',(-2.9,1.2,19.8));
#21203=CARTESIAN_POINT('',(-2.5,1.2,19.8));
#21204=CARTESIAN_POINT('',(-2.9,1.2,20.2));
#21205=CARTESIAN_POINT('',(-2.9,1.2,19.8));
#21206=CARTESIAN_POINT('',(-2.5,1.2,20.2));
#21207=CARTESIAN_POINT('',(-2.5,1.2,20.2));
#21208=CARTESIAN_POINT('',(-2.5,1.2,19.8));
#21209=CARTESIAN_POINT('Origin',(-2.5,-0.2,19.8));
#21210=CARTESIAN_POINT('',(-2.5,-0.2,19.8));
#21211=CARTESIAN_POINT('',(-2.5,-0.2,19.8));
#21212=CARTESIAN_POINT('',(-2.5,-0.2,20.2));
#21213=CARTESIAN_POINT('',(-2.5,-0.2,20.2));
#21214=CARTESIAN_POINT('',(-2.5,-0.2,19.8));
#21215=CARTESIAN_POINT('Origin',(-2.9,-0.2,19.8));
#21216=CARTESIAN_POINT('',(-2.9,-0.2,19.8));
#21217=CARTESIAN_POINT('',(-2.9,-0.2,19.8));
#21218=CARTESIAN_POINT('',(-2.9,-0.2,20.2));
#21219=CARTESIAN_POINT('',(-2.9,-0.2,20.2));
#21220=CARTESIAN_POINT('',(-2.9,-0.2,19.8));
#21221=CARTESIAN_POINT('Origin',(-2.9,1.2,19.8));
#21222=CARTESIAN_POINT('',(-2.9,1.2,19.8));
#21223=CARTESIAN_POINT('',(-2.9,1.2,20.2));
#21224=CARTESIAN_POINT('Origin',(-2.7,0.5,20.2));
#21225=CARTESIAN_POINT('Origin',(-2.7,0.5,19.8));
#21226=CARTESIAN_POINT('',(0.,0.,0.));
#21227=CARTESIAN_POINT('Origin',(-2.5,6.9,19.8));
#21228=CARTESIAN_POINT('',(-2.5,6.9,19.8));
#21229=CARTESIAN_POINT('',(-2.9,6.9,19.8));
#21230=CARTESIAN_POINT('',(-2.5,6.9,19.8));
#21231=CARTESIAN_POINT('',(-2.9,6.9,20.2));
#21232=CARTESIAN_POINT('',(-2.9,6.9,19.8));
#21233=CARTESIAN_POINT('',(-2.5,6.9,20.2));
#21234=CARTESIAN_POINT('',(-2.5,6.9,20.2));
#21235=CARTESIAN_POINT('',(-2.5,6.9,19.8));
#21236=CARTESIAN_POINT('Origin',(-2.5,5.5,19.8));
#21237=CARTESIAN_POINT('',(-2.5,5.5,19.8));
#21238=CARTESIAN_POINT('',(-2.5,5.5,19.8));
#21239=CARTESIAN_POINT('',(-2.5,5.5,20.2));
#21240=CARTESIAN_POINT('',(-2.5,5.5,20.2));
#21241=CARTESIAN_POINT('',(-2.5,5.5,19.8));
#21242=CARTESIAN_POINT('Origin',(-2.9,5.5,19.8));
#21243=CARTESIAN_POINT('',(-2.9,5.5,19.8));
#21244=CARTESIAN_POINT('',(-2.9,5.5,19.8));
#21245=CARTESIAN_POINT('',(-2.9,5.5,20.2));
#21246=CARTESIAN_POINT('',(-2.9,5.5,20.2));
#21247=CARTESIAN_POINT('',(-2.9,5.5,19.8));
#21248=CARTESIAN_POINT('Origin',(-2.9,6.9,19.8));
#21249=CARTESIAN_POINT('',(-2.9,6.9,19.8));
#21250=CARTESIAN_POINT('',(-2.9,6.9,20.2));
#21251=CARTESIAN_POINT('Origin',(-2.7,6.2,20.2));
#21252=CARTESIAN_POINT('Origin',(-2.7,6.2,19.8));
#21253=CARTESIAN_POINT('',(0.,0.,0.));
#21254=CARTESIAN_POINT('Origin',(-3.25,5.9,29.));
#21255=CARTESIAN_POINT('',(-3.5,6.,29.));
#21256=CARTESIAN_POINT('Origin',(-3.25,6.,29.));
#21257=CARTESIAN_POINT('',(-3.5,6.8,29.));
#21258=CARTESIAN_POINT('',(-3.5,5.9,29.));
#21259=CARTESIAN_POINT('Origin',(-3.25,6.8,29.));
#21260=CARTESIAN_POINT('Origin',(-2.47,4.9,19.8));
#21261=CARTESIAN_POINT('',(-2.47,5.,19.8));
#21262=CARTESIAN_POINT('',(-2.68431457505076,5.,19.8));
#21263=CARTESIAN_POINT('',(-2.86,5.,19.8));
#21264=CARTESIAN_POINT('',(-2.47,7.5,19.8));
#21265=CARTESIAN_POINT('',(-2.47,4.9,19.8));
#21266=CARTESIAN_POINT('',(-2.68431457505076,7.5,19.8));
#21267=CARTESIAN_POINT('',(-2.86,7.5,19.8));
#21268=CARTESIAN_POINT('',(-2.68431457505076,5.,19.8));
#21269=CARTESIAN_POINT('Origin',(-2.47,4.9,20.2));
#21270=CARTESIAN_POINT('',(-2.47,5.,20.2));
#21271=CARTESIAN_POINT('',(-2.47,5.,20.1));
#21272=CARTESIAN_POINT('',(-2.47,7.5,20.2));
#21273=CARTESIAN_POINT('',(-2.47,4.9,20.2));
#21274=CARTESIAN_POINT('',(-2.47,7.5,20.1));
#21275=CARTESIAN_POINT('Origin',(-2.9,4.9,20.2));
#21276=CARTESIAN_POINT('',(-2.68431457505076,5.,20.2));
#21277=CARTESIAN_POINT('',(-3.075,5.,20.2));
#21278=CARTESIAN_POINT('',(-2.68431457505076,7.5,20.2));
#21279=CARTESIAN_POINT('',(-2.68431457505076,5.,20.2));
#21280=CARTESIAN_POINT('',(-3.075,7.5,20.2));
#21281=CARTESIAN_POINT('Origin',(-3.25,7.5,20.));
#21282=CARTESIAN_POINT('',(-4.55,7.5,20.));
#21283=CARTESIAN_POINT('Origin',(-3.25,7.5,20.));
#21284=CARTESIAN_POINT('Origin',(-3.25,7.5,20.));
#21285=CARTESIAN_POINT('Origin',(-3.25,5.,20.));
#21286=CARTESIAN_POINT('Origin',(-3.25,5.,20.));
#21287=CARTESIAN_POINT('Origin',(-3.25,6.,29.));
#21288=CARTESIAN_POINT('',(-2.75,6.8,28.2516685226452));
#21289=CARTESIAN_POINT('',(-2.75,6.,28.2516685226452));
#21290=CARTESIAN_POINT('',(-2.75,6.,28.2516685226452));
#21291=CARTESIAN_POINT('',(-3.75,6.8,28.2516685226452));
#21292=CARTESIAN_POINT('Origin',(-3.25,6.8,29.));
#21293=CARTESIAN_POINT('',(-3.75,6.,28.2516685226452));
#21294=CARTESIAN_POINT('',(-3.75,6.,28.2516685226452));
#21295=CARTESIAN_POINT('Origin',(-3.25,6.,29.));
#21296=CARTESIAN_POINT('Origin',(-2.75,6.,29.));
#21297=CARTESIAN_POINT('',(-2.75,6.,21.2));
#21298=CARTESIAN_POINT('',(-2.75,6.,20.));
#21299=CARTESIAN_POINT('',(-2.75,6.8,21.2));
#21300=CARTESIAN_POINT('',(-2.75,5.,21.2));
#21301=CARTESIAN_POINT('',(-2.75,6.8,20.));
#21302=CARTESIAN_POINT('Origin',(-3.25,6.,24.5));
#21303=CARTESIAN_POINT('',(-3.75,6.,21.2));
#21304=CARTESIAN_POINT('',(-3.75,6.,29.));
#21305=CARTESIAN_POINT('Origin',(-3.25,6.,20.));
#21306=CARTESIAN_POINT('Origin',(-3.75,6.,20.));
#21307=CARTESIAN_POINT('',(-3.75,6.8,21.2));
#21308=CARTESIAN_POINT('',(-3.75,6.8,29.));
#21309=CARTESIAN_POINT('',(-3.75,5.,21.2));
#21310=CARTESIAN_POINT('Origin',(-3.25,6.8,24.5));
#21311=CARTESIAN_POINT('Origin',(-3.25,6.8,20.));
#21312=CARTESIAN_POINT('Origin',(-3.25,5.,20.));
#21313=CARTESIAN_POINT('',(-4.55,5.,20.));
#21314=CARTESIAN_POINT('',(-4.55,5.,20.));
#21315=CARTESIAN_POINT('Origin',(-3.25,5.,20.));
#21316=CARTESIAN_POINT('Origin',(-3.25,5.,20.));
#21317=CARTESIAN_POINT('',(0.,0.,0.));
#21318=CARTESIAN_POINT('Origin',(-3.25,6.8,29.));
#21319=CARTESIAN_POINT('',(-3.58,8.4,29.));
#21320=CARTESIAN_POINT('Origin',(-3.25,8.4,29.));
#21321=CARTESIAN_POINT('',(-3.58,6.8,29.));
#21322=CARTESIAN_POINT('',(-3.58,6.8,29.));
#21323=CARTESIAN_POINT('Origin',(-3.25,6.8,29.));
#21324=CARTESIAN_POINT('Origin',(-3.25,6.8,29.));
#21325=CARTESIAN_POINT('',(-3.65,8.4,29.));
#21326=CARTESIAN_POINT('Origin',(-3.25,8.4,29.));
#21327=CARTESIAN_POINT('',(-3.65,6.8,29.));
#21328=CARTESIAN_POINT('',(-3.65,6.8,29.));
#21329=CARTESIAN_POINT('Origin',(-3.25,6.8,29.));
#21330=CARTESIAN_POINT('Origin',(-3.25,8.4,29.));
#21331=CARTESIAN_POINT('Origin',(-3.25,6.8,29.));
#21332=CARTESIAN_POINT('',(0.,0.,0.));
#21333=CARTESIAN_POINT('Origin',(-3.25,-5.7,20.));
#21334=CARTESIAN_POINT('',(-3.475,-5.5,20.));
#21335=CARTESIAN_POINT('Origin',(-3.25,-5.5,20.));
#21336=CARTESIAN_POINT('',(-3.475,-5.7,20.));
#21337=CARTESIAN_POINT('',(-3.475,-5.7,20.));
#21338=CARTESIAN_POINT('Origin',(-3.25,-5.7,20.));
#21339=CARTESIAN_POINT('Origin',(-3.25,-5.7,20.));
#21340=CARTESIAN_POINT('',(-4.25,-5.5,20.));
#21341=CARTESIAN_POINT('Origin',(-3.25,-5.5,20.));
#21342=CARTESIAN_POINT('',(-4.25,-5.7,20.));
#21343=CARTESIAN_POINT('',(-4.25,-5.7,20.));
#21344=CARTESIAN_POINT('Origin',(-3.25,-5.7,20.));
#21345=CARTESIAN_POINT('Origin',(-3.25,-5.5,20.));
#21346=CARTESIAN_POINT('Origin',(-3.25,-5.7,20.));
#21347=CARTESIAN_POINT('',(0.,0.,0.));
#21348=CARTESIAN_POINT('Origin',(-3.25,7.5,20.));
#21349=CARTESIAN_POINT('',(-3.475,7.7,20.));
#21350=CARTESIAN_POINT('Origin',(-3.25,7.7,20.));
#21351=CARTESIAN_POINT('',(-3.475,7.5,20.));
#21352=CARTESIAN_POINT('',(-3.475,7.5,20.));
#21353=CARTESIAN_POINT('Origin',(-3.25,7.5,20.));
#21354=CARTESIAN_POINT('Origin',(-3.25,7.5,20.));
#21355=CARTESIAN_POINT('',(-4.25,7.7,20.));
#21356=CARTESIAN_POINT('Origin',(-3.25,7.7,20.));
#21357=CARTESIAN_POINT('',(-4.25,7.5,20.));
#21358=CARTESIAN_POINT('',(-4.25,7.5,20.));
#21359=CARTESIAN_POINT('Origin',(-3.25,7.5,20.));
#21360=CARTESIAN_POINT('Origin',(-3.25,7.7,20.));
#21361=CARTESIAN_POINT('Origin',(-3.25,7.5,20.));
#21362=CARTESIAN_POINT('',(0.,0.,0.));
#21363=CARTESIAN_POINT('Origin',(0.2,0.,0.));
#21364=CARTESIAN_POINT('',(0.2,2.2,-0.78));
#21365=CARTESIAN_POINT('',(0.2,2.2,-0.565685424949238));
#21366=CARTESIAN_POINT('',(0.2,2.2,0.));
#21367=CARTESIAN_POINT('',(0.2,-1.,-0.78));
#21368=CARTESIAN_POINT('',(0.2,0.,-0.78));
#21369=CARTESIAN_POINT('',(0.2,-1.,-0.565685424949238));
#21370=CARTESIAN_POINT('',(0.2,-1.,0.));
#21371=CARTESIAN_POINT('',(0.2,0.,-0.565685424949238));
#21372=CARTESIAN_POINT('Origin',(0.2,0.,-0.78));
#21373=CARTESIAN_POINT('',(-0.2,2.2,-0.78));
#21374=CARTESIAN_POINT('',(0.1,2.2,-0.78));
#21375=CARTESIAN_POINT('',(-0.2,-1.,-0.78));
#21376=CARTESIAN_POINT('',(-0.2,0.,-0.78));
#21377=CARTESIAN_POINT('',(0.1,-1.,-0.78));
#21378=CARTESIAN_POINT('Origin',(-0.2,0.,-0.78));
#21379=CARTESIAN_POINT('',(-0.2,2.2,-0.565685424949238));
#21380=CARTESIAN_POINT('',(-0.2,2.2,-0.39));
#21381=CARTESIAN_POINT('',(-0.2,-1.,-0.565685424949238));
#21382=CARTESIAN_POINT('',(-0.2,0.,-0.565685424949238));
#21383=CARTESIAN_POINT('',(-0.2,-1.,-0.39));
#21384=CARTESIAN_POINT('Origin',(0.,-1.,0.));
#21385=CARTESIAN_POINT('',(1.60662857109684,-1.,0.693717979106306));
#21386=CARTESIAN_POINT('',(1.5055822144029,-1.,0.892032620296856));
#21387=CARTESIAN_POINT('Origin',(0.,-1.,0.));
#21388=CARTESIAN_POINT('',(1.81978687191668,-1.,1.23627494547115));
#21389=CARTESIAN_POINT('Ctrl Pts',(1.5055822144029,-1.,0.892032620296856));
#21390=CARTESIAN_POINT('Ctrl Pts',(1.50980486806688,-1.,0.894452006964544));
#21391=CARTESIAN_POINT('Ctrl Pts',(1.51805569590094,-1.,0.899185047483511));
#21392=CARTESIAN_POINT('Ctrl Pts',(1.52984849887993,-1.,0.905967409625651));
#21393=CARTESIAN_POINT('Ctrl Pts',(1.54440491149498,-1.,0.914375919026456));
#21394=CARTESIAN_POINT('Ctrl Pts',(1.56065988578893,-1.,0.923832188944341));
#21395=CARTESIAN_POINT('Ctrl Pts',(1.57499388382243,-1.,0.932246680108685));
#21396=CARTESIAN_POINT('Ctrl Pts',(1.58744937487176,-1.,0.939646377893399));
#21397=CARTESIAN_POINT('Ctrl Pts',(1.59810042043673,-1.,0.946078063315257));
#21398=CARTESIAN_POINT('Ctrl Pts',(1.60706069896936,-1.,0.951613284356035));
#21399=CARTESIAN_POINT('Ctrl Pts',(1.61449324337085,-1.,0.956354422920671));
#21400=CARTESIAN_POINT('Ctrl Pts',(1.62061638140221,-1.,0.960438326101729));
#21401=CARTESIAN_POINT('Ctrl Pts',(1.62571930670187,-1.,0.964046107040536));
#21402=CARTESIAN_POINT('Ctrl Pts',(1.63013849959461,-1.,0.967387853230345));
#21403=CARTESIAN_POINT('Ctrl Pts',(1.63420665729798,-1.,0.970669715997509));
#21404=CARTESIAN_POINT('Ctrl Pts',(1.63820952658144,-1.,0.974066058287419));
#21405=CARTESIAN_POINT('Ctrl Pts',(1.64233990826687,-1.,0.977689794119417));
#21406=CARTESIAN_POINT('Ctrl Pts',(1.64665139190656,-1.,0.981562530939489));
#21407=CARTESIAN_POINT('Ctrl Pts',(1.65110016612638,-1.,0.985642622920821));
#21408=CARTESIAN_POINT('Ctrl Pts',(1.65559044289699,-1.,0.989855627854165));
#21409=CARTESIAN_POINT('Ctrl Pts',(1.66001553809947,-1.,0.994121836661306));
#21410=CARTESIAN_POINT('Ctrl Pts',(1.66430758030376,-1.,0.998389654952758));
#21411=CARTESIAN_POINT('Ctrl Pts',(1.66846059277303,-1.,1.00265091003727));
#21412=CARTESIAN_POINT('Ctrl Pts',(1.67250335383293,-1.,1.00692206696414));
#21413=CARTESIAN_POINT('Ctrl Pts',(1.67648246776464,-1.,1.01123236493511));
#21414=CARTESIAN_POINT('Ctrl Pts',(1.68044289894798,-1.,1.01561026162773));
#21415=CARTESIAN_POINT('Ctrl Pts',(1.68440578021706,-1.,1.02006795074201));
#21416=CARTESIAN_POINT('Ctrl Pts',(1.68836910178447,-1.,1.02460180535255));
#21417=CARTESIAN_POINT('Ctrl Pts',(1.69231840863458,-1.,1.02919977579147));
#21418=CARTESIAN_POINT('Ctrl Pts',(1.69623414782771,-1.,1.03384646003588));
#21419=CARTESIAN_POINT('Ctrl Pts',(1.70010052930962,-1.,1.03852922490789));
#21420=CARTESIAN_POINT('Ctrl Pts',(1.70391338707982,-1.,1.04324363334554));
#21421=CARTESIAN_POINT('Ctrl Pts',(1.70767646263649,-1.,1.04799085404995));
#21422=CARTESIAN_POINT('Ctrl Pts',(1.71139783543989,-1.,1.05277517202855));
#21423=CARTESIAN_POINT('Ctrl Pts',(1.7150865442702,-1.,1.05760163192479));
#21424=CARTESIAN_POINT('Ctrl Pts',(1.71874858456904,-1.,1.06247324680647));
#21425=CARTESIAN_POINT('Ctrl Pts',(1.72238500928453,-1.,1.06738966975462));
#21426=CARTESIAN_POINT('Ctrl Pts',(1.72599406198488,-1.,1.07234866990252));
#21427=CARTESIAN_POINT('Ctrl Pts',(1.72957248977424,-1.,1.0773470373727));
#21428=CARTESIAN_POINT('Ctrl Pts',(1.73311705663407,-1.,1.08238162784749));
#21429=CARTESIAN_POINT('Ctrl Pts',(1.73662628326091,-1.,1.08745056285427));
#21430=CARTESIAN_POINT('Ctrl Pts',(1.74010053962247,-1.,1.09255329056493));
#21431=CARTESIAN_POINT('Ctrl Pts',(1.74354119236208,-1.,1.09768999241226));
#21432=CARTESIAN_POINT('Ctrl Pts',(1.74695004214923,-1.,1.10286118991143));
#21433=CARTESIAN_POINT('Ctrl Pts',(1.7503286607592,-1.,1.10806728183007));
#21434=CARTESIAN_POINT('Ctrl Pts',(1.7536777209463,-1.,1.11330807582551));
#21435=CARTESIAN_POINT('Ctrl Pts',(1.75699720772105,-1.,1.11858293216763));
#21436=CARTESIAN_POINT('Ctrl Pts',(1.76028671825096,-1.,1.12389096855086));
#21437=CARTESIAN_POINT('Ctrl Pts',(1.7635457196617,-1.,1.12923123555075));
#21438=CARTESIAN_POINT('Ctrl Pts',(1.76677384551862,-1.,1.1346029180462));
#21439=CARTESIAN_POINT('Ctrl Pts',(1.76997111386769,-1.,1.14000548336975));
#21440=CARTESIAN_POINT('Ctrl Pts',(1.77313777896194,-1.,1.1454385822692));
#21441=CARTESIAN_POINT('Ctrl Pts',(1.7762742255701,-1.,1.15090197841515));
#21442=CARTESIAN_POINT('Ctrl Pts',(1.77938085564275,-1.,1.15639547194698));
#21443=CARTESIAN_POINT('Ctrl Pts',(1.78245795881009,-1.,1.16191881298499));
#21444=CARTESIAN_POINT('Ctrl Pts',(1.78550566040443,-1.,1.16747166312303));
#21445=CARTESIAN_POINT('Ctrl Pts',(1.78852398877616,-1.,1.17305363177328));
#21446=CARTESIAN_POINT('Ctrl Pts',(1.79151291552689,-1.,1.17866429440809));
#21447=CARTESIAN_POINT('Ctrl Pts',(1.79447240321515,-1.,1.18430321697432));
#21448=CARTESIAN_POINT('Ctrl Pts',(1.79740245923478,-1.,1.18996997934445));
#21449=CARTESIAN_POINT('Ctrl Pts',(1.80030314369879,-1.,1.19566418930242));
#21450=CARTESIAN_POINT('Ctrl Pts',(1.80317454838603,-1.,1.20138548938974));
#21451=CARTESIAN_POINT('Ctrl Pts',(1.80601678480707,-1.,1.20713356605475));
#21452=CARTESIAN_POINT('Ctrl Pts',(1.80882996917129,-1.,1.21290815708314));
#21453=CARTESIAN_POINT('Ctrl Pts',(1.81161420806656,-1.,1.21870906103557));
#21454=CARTESIAN_POINT('Ctrl Pts',(1.81436959210434,-1.,1.2245361330495));
#21455=CARTESIAN_POINT('Ctrl Pts',(1.8165508718364,-1.,1.2292186489137));
#21456=CARTESIAN_POINT('Ctrl Pts',(1.81817389921279,-1.,1.2327422452705));
#21457=CARTESIAN_POINT('Ctrl Pts',(1.81925017193666,-1.,1.23509651170476));
#21458=CARTESIAN_POINT('Ctrl Pts',(1.81978687191668,-1.,1.23627494547115));
#21459=CARTESIAN_POINT('',(1.73811241238545,-1.,1.34869019493419));
#21460=CARTESIAN_POINT('',(1.81978687191668,-1.,1.23627494547115));
#21461=CARTESIAN_POINT('',(1.31362392696032,-1.,1.15624053661742));
#21462=CARTESIAN_POINT('Ctrl Pts',(1.73811241238545,-1.,1.34869019493419));
#21463=CARTESIAN_POINT('Ctrl Pts',(1.73682580585691,-1.,1.34854391898045));
#21464=CARTESIAN_POINT('Ctrl Pts',(1.73425417885907,-1.,1.34824783112887));
#21465=CARTESIAN_POINT('Ctrl Pts',(1.7304014965394,-1.,1.34779309152035));
#21466=CARTESIAN_POINT('Ctrl Pts',(1.72527410680674,-1.,1.34716554819527));
#21467=CARTESIAN_POINT('Ctrl Pts',(1.7188807715049,-1.,1.34634568653227));
#21468=CARTESIAN_POINT('Ctrl Pts',(1.71250340686822,-1.,1.34549029589416));
#21469=CARTESIAN_POINT('Ctrl Pts',(1.70614212266738,-1.,1.34459924533831));
#21470=CARTESIAN_POINT('Ctrl Pts',(1.69979707754427,-1.,1.34367237124483));
#21471=CARTESIAN_POINT('Ctrl Pts',(1.6934684849687,-1.,1.34270948206319));
#21472=CARTESIAN_POINT('Ctrl Pts',(1.68715660868764,-1.,1.341710374848));
#21473=CARTESIAN_POINT('Ctrl Pts',(1.68086176030362,-1.,1.34067485185203));
#21474=CARTESIAN_POINT('Ctrl Pts',(1.67458429426086,-1.,1.3396027347034));
#21475=CARTESIAN_POINT('Ctrl Pts',(1.66832460783989,-1.,1.33849388654388));
#21476=CARTESIAN_POINT('Ctrl Pts',(1.66208312541983,-1.,1.33734820885262));
#21477=CARTESIAN_POINT('Ctrl Pts',(1.65586025952593,-1.,1.33616559745172));
#21478=CARTESIAN_POINT('Ctrl Pts',(1.6496563728683,-1.,1.33494590467993));
#21479=CARTESIAN_POINT('Ctrl Pts',(1.6434717485603,-1.,1.33368890676572));
#21480=CARTESIAN_POINT('Ctrl Pts',(1.63730653475089,-1.,1.33239425103724));
#21481=CARTESIAN_POINT('Ctrl Pts',(1.63116079730923,-1.,1.33106149345645));
#21482=CARTESIAN_POINT('Ctrl Pts',(1.62503464209797,-1.,1.3296901950568));
#21483=CARTESIAN_POINT('Ctrl Pts',(1.61892832270724,-1.,1.32828000610449));
#21484=CARTESIAN_POINT('Ctrl Pts',(1.6128423401575,-1.,1.32683074483356));
#21485=CARTESIAN_POINT('Ctrl Pts',(1.60677758290954,-1.,1.32534250785782));
#21486=CARTESIAN_POINT('Ctrl Pts',(1.60073511858687,-1.,1.32381550858256));
#21487=CARTESIAN_POINT('Ctrl Pts',(1.59471591079403,-1.,1.32224985747682));
#21488=CARTESIAN_POINT('Ctrl Pts',(1.58872057258245,-1.,1.32064537110892));
#21489=CARTESIAN_POINT('Ctrl Pts',(1.58274907898834,-1.,1.31900135021432));
#21490=CARTESIAN_POINT('Ctrl Pts',(1.5768005650559,-1.,1.31731642317187));
#21491=CARTESIAN_POINT('Ctrl Pts',(1.57087397835723,-1.,1.31558903860016));
#21492=CARTESIAN_POINT('Ctrl Pts',(1.56496872402353,-1.,1.31381795281002));
#21493=CARTESIAN_POINT('Ctrl Pts',(1.55908521254821,-1.,1.31200264341696));
#21494=CARTESIAN_POINT('Ctrl Pts',(1.55322568759481,-1.,1.31014393684222));
#21495=CARTESIAN_POINT('Ctrl Pts',(1.54739413957185,-1.,1.30824393907473));
#21496=CARTESIAN_POINT('Ctrl Pts',(1.54159462645432,-1.,1.30630475189556));
#21497=CARTESIAN_POINT('Ctrl Pts',(1.53582981268977,-1.,1.30432735639489));
#21498=CARTESIAN_POINT('Ctrl Pts',(1.53009970283891,-1.,1.30231064395568));
#21499=CARTESIAN_POINT('Ctrl Pts',(1.52439957861062,-1.,1.30024984366328));
#21500=CARTESIAN_POINT('Ctrl Pts',(1.51872184912724,-1.,1.29813791800747));
#21501=CARTESIAN_POINT('Ctrl Pts',(1.51305994241402,-1.,1.29596850710509));
#21502=CARTESIAN_POINT('Ctrl Pts',(1.50741159078365,-1.,1.29373841372842));
#21503=CARTESIAN_POINT('Ctrl Pts',(1.50178230149776,-1.,1.29145022885181));
#21504=CARTESIAN_POINT('Ctrl Pts',(1.49618896881754,-1.,1.28911506584254));
#21505=CARTESIAN_POINT('Ctrl Pts',(1.4906522831278,-1.,1.2867467611644));
#21506=CARTESIAN_POINT('Ctrl Pts',(1.4851881711891,-1.,1.28435533880201));
#21507=CARTESIAN_POINT('Ctrl Pts',(1.47980070347095,-1.,1.28194158939517));
#21508=CARTESIAN_POINT('Ctrl Pts',(1.4744717526707,-1.,1.2794891824849));
#21509=CARTESIAN_POINT('Ctrl Pts',(1.46916035917133,-1.,1.2769641483109));
#21510=CARTESIAN_POINT('Ctrl Pts',(1.46382431332476,-1.,1.27433119897822));
#21511=CARTESIAN_POINT('Ctrl Pts',(1.45843906294697,-1.,1.27156805265289));
#21512=CARTESIAN_POINT('Ctrl Pts',(1.45301422764247,-1.,1.2686778680489));
#21513=CARTESIAN_POINT('Ctrl Pts',(1.44761985001662,-1.,1.26570925118868));
#21514=CARTESIAN_POINT('Ctrl Pts',(1.44236470511303,-1.,1.26273903323859));
#21515=CARTESIAN_POINT('Ctrl Pts',(1.43734919180847,-1.,1.25983531012005));
#21516=CARTESIAN_POINT('Ctrl Pts',(1.43262645609691,-1.,1.25702687965755));
#21517=CARTESIAN_POINT('Ctrl Pts',(1.42815938799387,-1.,1.25426945222639));
#21518=CARTESIAN_POINT('Ctrl Pts',(1.42378102115575,-1.,1.2514145557001));
#21519=CARTESIAN_POINT('Ctrl Pts',(1.41923722596025,-1.,1.24824430986571));
#21520=CARTESIAN_POINT('Ctrl Pts',(1.41422913175179,-1.,1.24450600513056));
#21521=CARTESIAN_POINT('Ctrl Pts',(1.40845295531283,-1.,1.23994455029534));
#21522=CARTESIAN_POINT('Ctrl Pts',(1.40164708206106,-1.,1.23434087290423));
#21523=CARTESIAN_POINT('Ctrl Pts',(1.39361389568796,-1.,1.22752961899387));
#21524=CARTESIAN_POINT('Ctrl Pts',(1.38420564527715,-1.,1.21938737280852));
#21525=CARTESIAN_POINT('Ctrl Pts',(1.37331915607905,-1.,1.20982812925645));
#21526=CARTESIAN_POINT('Ctrl Pts',(1.36088705043885,-1.,1.1987959077932));
#21527=CARTESIAN_POINT('Ctrl Pts',(1.34687054001093,-1.,1.18625865667441));
#21528=CARTESIAN_POINT('Ctrl Pts',(1.33437539347008,-1.,1.17501305789857));
#21529=CARTESIAN_POINT('Ctrl Pts',(1.32428080721772,-1.,1.16589330093588));
#21530=CARTESIAN_POINT('Ctrl Pts',(1.31722977216397,-1.,1.15950888730809));
#21531=CARTESIAN_POINT('Ctrl Pts',(1.31362392696032,-1.,1.15624053661742));
#21532=CARTESIAN_POINT('',(1.15624053661742,-1.,1.31362392696033));
#21533=CARTESIAN_POINT('Origin',(0.,-1.,0.));
#21534=CARTESIAN_POINT('',(1.34869019493419,-1.,1.73811241238545));
#21535=CARTESIAN_POINT('Ctrl Pts',(1.15624053661742,-1.,1.31362392696033));
#21536=CARTESIAN_POINT('Ctrl Pts',(1.15950888730433,-1.,1.3172297721596));
#21537=CARTESIAN_POINT('Ctrl Pts',(1.16589330092532,-1.,1.32428080720544));
#21538=CARTESIAN_POINT('Ctrl Pts',(1.17501305787994,-1.,1.33437539344842));
#21539=CARTESIAN_POINT('Ctrl Pts',(1.18625865664915,-1.,1.34687053998157));
#21540=CARTESIAN_POINT('Ctrl Pts',(1.1987959077656,-1.,1.36088705040677));
#21541=CARTESIAN_POINT('Ctrl Pts',(1.20982812923113,-1.,1.37331915604962));
#21542=CARTESIAN_POINT('Ctrl Pts',(1.21938737278853,-1.,1.38420564525391));
#21543=CARTESIAN_POINT('Ctrl Pts',(1.22752961898063,-1.,1.39361389567257));
#21544=CARTESIAN_POINT('Ctrl Pts',(1.23434087289768,-1.,1.40164708205345));
#21545=CARTESIAN_POINT('Ctrl Pts',(1.23994455029421,-1.,1.40845295531151));
#21546=CARTESIAN_POINT('Ctrl Pts',(1.24450600513278,-1.,1.41422913175437));
#21547=CARTESIAN_POINT('Ctrl Pts',(1.24824430986911,-1.,1.41923722596421));
#21548=CARTESIAN_POINT('Ctrl Pts',(1.25141455570299,-1.,1.42378102115911));
#21549=CARTESIAN_POINT('Ctrl Pts',(1.25426945222783,-1.,1.42815938799555));
#21550=CARTESIAN_POINT('Ctrl Pts',(1.25702687965744,-1.,1.43262645609679));
#21551=CARTESIAN_POINT('Ctrl Pts',(1.25983531011894,-1.,1.43734919180719));
#21552=CARTESIAN_POINT('Ctrl Pts',(1.26273903323723,-1.,1.44236470511145));
#21553=CARTESIAN_POINT('Ctrl Pts',(1.26570925118767,-1.,1.44761985001544));
#21554=CARTESIAN_POINT('Ctrl Pts',(1.26867786804854,-1.,1.45301422764205));
#21555=CARTESIAN_POINT('Ctrl Pts',(1.27156805265312,-1.,1.45843906294725));
#21556=CARTESIAN_POINT('Ctrl Pts',(1.27433119897877,-1.,1.4638243133254));
#21557=CARTESIAN_POINT('Ctrl Pts',(1.27696414831144,-1.,1.46916035917197));
#21558=CARTESIAN_POINT('Ctrl Pts',(1.27948918248524,-1.,1.4744717526711));
#21559=CARTESIAN_POINT('Ctrl Pts',(1.28194158939522,-1.,1.47980070347102));
#21560=CARTESIAN_POINT('Ctrl Pts',(1.28435533880184,-1.,1.48518817118891));
#21561=CARTESIAN_POINT('Ctrl Pts',(1.28674676116415,-1.,1.4906522831275));
#21562=CARTESIAN_POINT('Ctrl Pts',(1.28911506584232,-1.,1.49618896881729));
#21563=CARTESIAN_POINT('Ctrl Pts',(1.29145022885171,-1.,1.50178230149764));
#21564=CARTESIAN_POINT('Ctrl Pts',(1.29373841372843,-1.,1.50741159078367));
#21565=CARTESIAN_POINT('Ctrl Pts',(1.29596850710518,-1.,1.51305994241412));
#21566=CARTESIAN_POINT('Ctrl Pts',(1.29813791800757,-1.,1.51872184912735));
#21567=CARTESIAN_POINT('Ctrl Pts',(1.30024984366334,-1.,1.5243995786107));
#21568=CARTESIAN_POINT('Ctrl Pts',(1.3023106439557,-1.,1.53009970283893));
#21569=CARTESIAN_POINT('Ctrl Pts',(1.30432735639487,-1.,1.53582981268976));
#21570=CARTESIAN_POINT('Ctrl Pts',(1.30630475189553,-1.,1.54159462645428));
#21571=CARTESIAN_POINT('Ctrl Pts',(1.30824393907471,-1.,1.54739413957183));
#21572=CARTESIAN_POINT('Ctrl Pts',(1.31014393684221,-1.,1.55322568759481));
#21573=CARTESIAN_POINT('Ctrl Pts',(1.31200264341696,-1.,1.55908521254822));
#21574=CARTESIAN_POINT('Ctrl Pts',(1.31381795281002,-1.,1.56496872402352));
#21575=CARTESIAN_POINT('Ctrl Pts',(1.31558903860015,-1.,1.57087397835721));
#21576=CARTESIAN_POINT('Ctrl Pts',(1.31731642317183,-1.,1.57680056505585));
#21577=CARTESIAN_POINT('Ctrl Pts',(1.31900135021428,-1.,1.58274907898829));
#21578=CARTESIAN_POINT('Ctrl Pts',(1.32064537110891,-1.,1.58872057258244));
#21579=CARTESIAN_POINT('Ctrl Pts',(1.32224985747686,-1.,1.59471591079408));
#21580=CARTESIAN_POINT('Ctrl Pts',(1.32381550858266,-1.,1.600735118587));
#21581=CARTESIAN_POINT('Ctrl Pts',(1.32534250785794,-1.,1.6067775829097));
#21582=CARTESIAN_POINT('Ctrl Pts',(1.32683074483365,-1.,1.61284234015762));
#21583=CARTESIAN_POINT('Ctrl Pts',(1.32828000610448,-1.,1.61892832270723));
#21584=CARTESIAN_POINT('Ctrl Pts',(1.32969019505665,-1.,1.62503464209777));
#21585=CARTESIAN_POINT('Ctrl Pts',(1.33106149345618,-1.,1.63116079730887));
#21586=CARTESIAN_POINT('Ctrl Pts',(1.33239425103694,-1.,1.6373065347505));
#21587=CARTESIAN_POINT('Ctrl Pts',(1.33368890676554,-1.,1.64347174856007));
#21588=CARTESIAN_POINT('Ctrl Pts',(1.33494590468003,-1.,1.64965637286843));
#21589=CARTESIAN_POINT('Ctrl Pts',(1.33616559745217,-1.,1.65586025952651));
#21590=CARTESIAN_POINT('Ctrl Pts',(1.33734820885331,-1.,1.66208312542073));
#21591=CARTESIAN_POINT('Ctrl Pts',(1.33849388654458,-1.,1.66832460784078));
#21592=CARTESIAN_POINT('Ctrl Pts',(1.33960273470372,-1.,1.67458429426126));
#21593=CARTESIAN_POINT('Ctrl Pts',(1.3406748518516,-1.,1.68086176030308));
#21594=CARTESIAN_POINT('Ctrl Pts',(1.34171037484673,-1.,1.68715660868602));
#21595=CARTESIAN_POINT('Ctrl Pts',(1.34270948206139,-1.,1.6934684849664));
#21596=CARTESIAN_POINT('Ctrl Pts',(1.34367237124322,-1.,1.69979707754221));
#21597=CARTESIAN_POINT('Ctrl Pts',(1.34459924533783,-1.,1.70614212266676));
#21598=CARTESIAN_POINT('Ctrl Pts',(1.34549029589563,-1.,1.71250340687011));
#21599=CARTESIAN_POINT('Ctrl Pts',(1.34634568653586,-1.,1.7188807715095));
#21600=CARTESIAN_POINT('Ctrl Pts',(1.34716554820013,-1.,1.72527410681298));
#21601=CARTESIAN_POINT('Ctrl Pts',(1.3477930915247,-1.,1.73040149654497));
#21602=CARTESIAN_POINT('Ctrl Pts',(1.34824783113158,-1.,1.73425417886255));
#21603=CARTESIAN_POINT('Ctrl Pts',(1.34854391898145,-1.,1.73682580585819));
#21604=CARTESIAN_POINT('Ctrl Pts',(1.34869019493419,-1.,1.73811241238545));
#21605=CARTESIAN_POINT('',(1.23627494547115,-1.,1.81978687191668));
#21606=CARTESIAN_POINT('',(1.34869019493419,-1.,1.73811241238545));
#21607=CARTESIAN_POINT('',(0.892032620296855,-1.,1.5055822144029));
#21608=CARTESIAN_POINT('Ctrl Pts',(1.23627494547115,-1.,1.81978687191668));
#21609=CARTESIAN_POINT('Ctrl Pts',(1.23509651170384,-1.,1.81925017193531));
#21610=CARTESIAN_POINT('Ctrl Pts',(1.23274224526804,-1.,1.81817389920914));
#21611=CARTESIAN_POINT('Ctrl Pts',(1.22921864890975,-1.,1.81655087183054));
#21612=CARTESIAN_POINT('Ctrl Pts',(1.22453613304507,-1.,1.81436959209778));
#21613=CARTESIAN_POINT('Ctrl Pts',(1.2187090610323,-1.,1.81161420806172));
#21614=CARTESIAN_POINT('Ctrl Pts',(1.2129081570818,-1.,1.80882996916931));
#21615=CARTESIAN_POINT('Ctrl Pts',(1.20713356605519,-1.,1.80601678480772));
#21616=CARTESIAN_POINT('Ctrl Pts',(1.2013854893912,-1.,1.8031745483882));
#21617=CARTESIAN_POINT('Ctrl Pts',(1.19566418930405,-1.,1.80030314370121));
#21618=CARTESIAN_POINT('Ctrl Pts',(1.1899699793456,-1.,1.79740245923649));
#21619=CARTESIAN_POINT('Ctrl Pts',(1.18430321697471,-1.,1.79447240321572));
#21620=CARTESIAN_POINT('Ctrl Pts',(1.17866429440781,-1.,1.79151291552646));
#21621=CARTESIAN_POINT('Ctrl Pts',(1.17305363177265,-1.,1.78852398877523));
#21622=CARTESIAN_POINT('Ctrl Pts',(1.16747166312239,-1.,1.78550566040349));
#21623=CARTESIAN_POINT('Ctrl Pts',(1.16191881298458,-1.,1.78245795880949));
#21624=CARTESIAN_POINT('Ctrl Pts',(1.15639547194689,-1.,1.77938085564261));
#21625=CARTESIAN_POINT('Ctrl Pts',(1.15090197841531,-1.,1.77627422557034));
#21626=CARTESIAN_POINT('Ctrl Pts',(1.14543858226948,-1.,1.77313777896234));
#21627=CARTESIAN_POINT('Ctrl Pts',(1.14000548337,-1.,1.76997111386806));
#21628=CARTESIAN_POINT('Ctrl Pts',(1.13460291804634,-1.,1.76677384551883));
#21629=CARTESIAN_POINT('Ctrl Pts',(1.12923123555076,-1.,1.76354571966171));
#21630=CARTESIAN_POINT('Ctrl Pts',(1.12389096855078,-1.,1.76028671825084));
#21631=CARTESIAN_POINT('Ctrl Pts',(1.11858293216752,-1.,1.75699720772089));
#21632=CARTESIAN_POINT('Ctrl Pts',(1.11330807582542,-1.,1.75367772094617));
#21633=CARTESIAN_POINT('Ctrl Pts',(1.10806728183003,-1.,1.75032866075914));
#21634=CARTESIAN_POINT('Ctrl Pts',(1.10286118991144,-1.,1.74695004214924));
#21635=CARTESIAN_POINT('Ctrl Pts',(1.09768999241229,-1.,1.74354119236212));
#21636=CARTESIAN_POINT('Ctrl Pts',(1.09255329056496,-1.,1.74010053962252));
#21637=CARTESIAN_POINT('Ctrl Pts',(1.08745056285429,-1.,1.73662628326093));
#21638=CARTESIAN_POINT('Ctrl Pts',(1.08238162784749,-1.,1.73311705663407));
#21639=CARTESIAN_POINT('Ctrl Pts',(1.0773470373727,-1.,1.72957248977424));
#21640=CARTESIAN_POINT('Ctrl Pts',(1.07234866990252,-1.,1.72599406198489));
#21641=CARTESIAN_POINT('Ctrl Pts',(1.06738966975463,-1.,1.72238500928456));
#21642=CARTESIAN_POINT('Ctrl Pts',(1.06247324680649,-1.,1.71874858456908));
#21643=CARTESIAN_POINT('Ctrl Pts',(1.05760163192481,-1.,1.71508654427022));
#21644=CARTESIAN_POINT('Ctrl Pts',(1.05277517202853,-1.,1.71139783543986));
#21645=CARTESIAN_POINT('Ctrl Pts',(1.0479908540499,-1.,1.70767646263641));
#21646=CARTESIAN_POINT('Ctrl Pts',(1.04324363334546,-1.,1.70391338707969));
#21647=CARTESIAN_POINT('Ctrl Pts',(1.03852922490782,-1.,1.70010052930951));
#21648=CARTESIAN_POINT('Ctrl Pts',(1.03384646003587,-1.,1.69623414782769));
#21649=CARTESIAN_POINT('Ctrl Pts',(1.02919977579155,-1.,1.69231840863471));
#21650=CARTESIAN_POINT('Ctrl Pts',(1.02460180535272,-1.,1.68836910178475));
#21651=CARTESIAN_POINT('Ctrl Pts',(1.02006795074222,-1.,1.68440578021739));
#21652=CARTESIAN_POINT('Ctrl Pts',(1.01561026162786,-1.,1.6804428989482));
#21653=CARTESIAN_POINT('Ctrl Pts',(1.01123236493507,-1.,1.67648246776457));
#21654=CARTESIAN_POINT('Ctrl Pts',(1.00692206696387,-1.,1.67250335383248));
#21655=CARTESIAN_POINT('Ctrl Pts',(1.00265091003682,-1.,1.66846059277231));
#21656=CARTESIAN_POINT('Ctrl Pts',(0.998389654952317,-1.,1.66430758030304));
#21657=CARTESIAN_POINT('Ctrl Pts',(0.994121836661115,-1.,1.66001553809916));
#21658=CARTESIAN_POINT('Ctrl Pts',(0.98985562785445,-1.,1.65559044289746));
#21659=CARTESIAN_POINT('Ctrl Pts',(0.985642622921626,-1.,1.6511001661277));
#21660=CARTESIAN_POINT('Ctrl Pts',(0.981562530940574,-1.,1.64665139190834));
#21661=CARTESIAN_POINT('Ctrl Pts',(0.977689794120296,-1.,1.64233990826831));
#21662=CARTESIAN_POINT('Ctrl Pts',(0.974066058287501,-1.,1.63820952658157));
#21663=CARTESIAN_POINT('Ctrl Pts',(0.970669715996356,-1.,1.63420665729609));
#21664=CARTESIAN_POINT('Ctrl Pts',(0.967387853228041,-1.,1.63013849959083));
#21665=CARTESIAN_POINT('Ctrl Pts',(0.964046107037821,-1.,1.6257193066974));
#21666=CARTESIAN_POINT('Ctrl Pts',(0.960438326099958,-1.,1.62061638139929));
#21667=CARTESIAN_POINT('Ctrl Pts',(0.956354422921572,-1.,1.61449324337233));
#21668=CARTESIAN_POINT('Ctrl Pts',(0.951613284361247,-1.,1.60706069897794));
#21669=CARTESIAN_POINT('Ctrl Pts',(0.946078063325795,-1.,1.59810042045408));
#21670=CARTESIAN_POINT('Ctrl Pts',(0.939646377909319,-1.,1.58744937489796));
#21671=CARTESIAN_POINT('Ctrl Pts',(0.932246680128848,-1.,1.57499388385561));
#21672=CARTESIAN_POINT('Ctrl Pts',(0.923832188966322,-1.,1.56065988582509));
#21673=CARTESIAN_POINT('Ctrl Pts',(0.914375919046579,-1.,1.54440491152808));
#21674=CARTESIAN_POINT('Ctrl Pts',(0.905967409640498,-1.,1.52984849890434));
#21675=CARTESIAN_POINT('Ctrl Pts',(0.89918504749193,-1.,1.51805569591479));
#21676=CARTESIAN_POINT('Ctrl Pts',(0.894452006967538,-1.,1.50980486807181));
#21677=CARTESIAN_POINT('Ctrl Pts',(0.892032620296855,-1.,1.5055822144029));
#21678=CARTESIAN_POINT('',(0.693717979106305,-1.,1.60662857109684));
#21679=CARTESIAN_POINT('Origin',(0.,-1.,0.));
#21680=CARTESIAN_POINT('',(0.7455743247944,-1.,2.0698113262342));
#21681=CARTESIAN_POINT('Ctrl Pts',(0.693717979106305,-1.,1.60662857109684));
#21682=CARTESIAN_POINT('Ctrl Pts',(0.69571209787897,-1.,1.61106790957619));
#21683=CARTESIAN_POINT('Ctrl Pts',(0.699605146398836,-1.,1.61974673471117));
#21684=CARTESIAN_POINT('Ctrl Pts',(0.705159151977294,-1.,1.6321654166204));
#21685=CARTESIAN_POINT('Ctrl Pts',(0.711993139340447,-1.,1.64752408828442));
#21686=CARTESIAN_POINT('Ctrl Pts',(0.719585433787949,-1.,1.66472880551777));
#21687=CARTESIAN_POINT('Ctrl Pts',(0.726235967982445,-1.,1.67996158451922));
#21688=CARTESIAN_POINT('Ctrl Pts',(0.731963238685357,-1.,1.69326921972915));
#21689=CARTESIAN_POINT('Ctrl Pts',(0.736799665716932,-1.,1.70473309004249));
#21690=CARTESIAN_POINT('Ctrl Pts',(0.74079516202821,-1.,1.71447789751001));
#21691=CARTESIAN_POINT('Ctrl Pts',(0.744021445433093,-1.,1.72268229916769));
#21692=CARTESIAN_POINT('Ctrl Pts',(0.746574710097752,-1.,1.72958533647714));
#21693=CARTESIAN_POINT('Ctrl Pts',(0.74858246295687,-1.,1.7355035168033));
#21694=CARTESIAN_POINT('Ctrl Pts',(0.750193435981249,-1.,1.74080458267114));
#21695=CARTESIAN_POINT('Ctrl Pts',(0.751555614164482,-1.,1.74585086852502));
#21696=CARTESIAN_POINT('Ctrl Pts',(0.752797683531314,-1.,1.75095139468794));
#21697=CARTESIAN_POINT('Ctrl Pts',(0.754009254027828,-1.,1.75631083600019));
#21698=CARTESIAN_POINT('Ctrl Pts',(0.755220979974461,-1.,1.76197817240128));
#21699=CARTESIAN_POINT('Ctrl Pts',(0.75642189602781,-1.,1.76789396002998));
#21700=CARTESIAN_POINT('Ctrl Pts',(0.757578264077028,-1.,1.77394167108292));
#21701=CARTESIAN_POINT('Ctrl Pts',(0.758650626677518,-1.,1.77999411220945));
#21702=CARTESIAN_POINT('Ctrl Pts',(0.759614401110189,-1.,1.78596964884604));
#21703=CARTESIAN_POINT('Ctrl Pts',(0.760469555880749,-1.,1.7918581561088));
#21704=CARTESIAN_POINT('Ctrl Pts',(0.761229695230558,-1.,1.79768986997783));
#21705=CARTESIAN_POINT('Ctrl Pts',(0.761915336443547,-1.,1.80351583877342));
#21706=CARTESIAN_POINT('Ctrl Pts',(0.762546129463938,-1.,1.80938551463965));
#21707=CARTESIAN_POINT('Ctrl Pts',(0.763132003836634,-1.,1.8153211840553));
#21708=CARTESIAN_POINT('Ctrl Pts',(0.763673465462726,-1.,1.82131873145266));
#21709=CARTESIAN_POINT('Ctrl Pts',(0.764165902605995,-1.,1.82735991200065));
#21710=CARTESIAN_POINT('Ctrl Pts',(0.764602549687853,-1.,1.83342077227142));
#21711=CARTESIAN_POINT('Ctrl Pts',(0.764978057881737,-1.,1.83948181064835));
#21712=CARTESIAN_POINT('Ctrl Pts',(0.765291664862029,-1.,1.84553698875924));
#21713=CARTESIAN_POINT('Ctrl Pts',(0.765545710619062,-1.,1.85158945130063));
#21714=CARTESIAN_POINT('Ctrl Pts',(0.765744212909318,-1.,1.85764741390394));
#21715=CARTESIAN_POINT('Ctrl Pts',(0.765891519092547,-1.,1.86372027063312));
#21716=CARTESIAN_POINT('Ctrl Pts',(0.765990708546091,-1.,1.86981398314341));
#21717=CARTESIAN_POINT('Ctrl Pts',(0.766042837036744,-1.,1.87592888967883));
#21718=CARTESIAN_POINT('Ctrl Pts',(0.766047794851864,-1.,1.88206215302561));
#21719=CARTESIAN_POINT('Ctrl Pts',(0.766004837062091,-1.,1.88820926433409));
#21720=CARTESIAN_POINT('Ctrl Pts',(0.765913193856978,-1.,1.89436577771388));
#21721=CARTESIAN_POINT('Ctrl Pts',(0.765772772593386,-1.,1.90052930393596));
#21722=CARTESIAN_POINT('Ctrl Pts',(0.765584196937919,-1.,1.90669961402356));
#21723=CARTESIAN_POINT('Ctrl Pts',(0.765348465884722,-1.,1.91287765805169));
#21724=CARTESIAN_POINT('Ctrl Pts',(0.765066729667088,-1.,1.91906491634196));
#21725=CARTESIAN_POINT('Ctrl Pts',(0.764740025488211,-1.,1.92526263537048));
#21726=CARTESIAN_POINT('Ctrl Pts',(0.76436901067394,-1.,1.93147105496382));
#21727=CARTESIAN_POINT('Ctrl Pts',(0.763954049121458,-1.,1.93768964875886));
#21728=CARTESIAN_POINT('Ctrl Pts',(0.763495333538629,-1.,1.9439174661764));
#21729=CARTESIAN_POINT('Ctrl Pts',(0.762992990878769,-1.,1.95015342590024));
#21730=CARTESIAN_POINT('Ctrl Pts',(0.762447203806178,-1.,1.95639665309869));
#21731=CARTESIAN_POINT('Ctrl Pts',(0.761858300014423,-1.,1.96264672744186));
#21732=CARTESIAN_POINT('Ctrl Pts',(0.76122669048382,-1.,1.96890351582499));
#21733=CARTESIAN_POINT('Ctrl Pts',(0.760552825409757,-1.,1.97516705321494));
#21734=CARTESIAN_POINT('Ctrl Pts',(0.75983714745219,-1.,1.98143741418172));
#21735=CARTESIAN_POINT('Ctrl Pts',(0.759080037802488,-1.,1.98771456680874));
#21736=CARTESIAN_POINT('Ctrl Pts',(0.758281796766761,-1.,1.99399831098817));
#21737=CARTESIAN_POINT('Ctrl Pts',(0.757442676862724,-1.,2.00028834739178));
#21738=CARTESIAN_POINT('Ctrl Pts',(0.75656290464667,-1.,2.0065843158773));
#21739=CARTESIAN_POINT('Ctrl Pts',(0.755642704957865,-1.,2.01288584328084));
#21740=CARTESIAN_POINT('Ctrl Pts',(0.754682330722816,-1.,2.01919259405809));
#21741=CARTESIAN_POINT('Ctrl Pts',(0.753682061112768,-1.,2.02550428623313));
#21742=CARTESIAN_POINT('Ctrl Pts',(0.75264218048721,-1.,2.03182068456221));
#21743=CARTESIAN_POINT('Ctrl Pts',(0.751562963361115,-1.,2.03814160092099));
#21744=CARTESIAN_POINT('Ctrl Pts',(0.750444657875575,-1.,2.04446689147979));
#21745=CARTESIAN_POINT('Ctrl Pts',(0.749287468665046,-1.,2.05079645592154));
#21746=CARTESIAN_POINT('Ctrl Pts',(0.748091554183802,-1.,2.05713023031007));
#21747=CARTESIAN_POINT('Ctrl Pts',(0.747103932787919,-1.,2.06220058927826));
#21748=CARTESIAN_POINT('Ctrl Pts',(0.7463458715442,-1.,2.06600523016815));
#21749=CARTESIAN_POINT('Ctrl Pts',(0.745832791378367,-1.,2.06854248895728));
#21750=CARTESIAN_POINT('Ctrl Pts',(0.7455743247944,-1.,2.0698113262342));
#21751=CARTESIAN_POINT('',(0.61342227326009,-1.,2.11275013067528));
#21752=CARTESIAN_POINT('',(0.7455743247944,-1.,2.0698113262342));
#21753=CARTESIAN_POINT('',(0.383122945602004,-1.,1.7075470150345));
#21754=CARTESIAN_POINT('Ctrl Pts',(0.61342227326009,-1.,2.11275013067528));
#21755=CARTESIAN_POINT('Ctrl Pts',(0.6124673655618,-1.,2.11187554259986));
#21756=CARTESIAN_POINT('Ctrl Pts',(0.610560911689898,-1.,2.11012443807238));
#21757=CARTESIAN_POINT('Ctrl Pts',(0.607711315454876,-1.,2.1074919961518));
#21758=CARTESIAN_POINT('Ctrl Pts',(0.60393203073603,-1.,2.10397049886949));
#21759=CARTESIAN_POINT('Ctrl Pts',(0.599241616420533,-1.,2.0995493086477));
#21760=CARTESIAN_POINT('Ctrl Pts',(0.594585006052162,-1.,2.0951087622027));
#21761=CARTESIAN_POINT('Ctrl Pts',(0.589962365403406,-1.,2.09064881812129));
#21762=CARTESIAN_POINT('Ctrl Pts',(0.585373918991617,-1.,2.08616943727951));
#21763=CARTESIAN_POINT('Ctrl Pts',(0.580819952108063,-1.,2.08167059018418));
#21764=CARTESIAN_POINT('Ctrl Pts',(0.576300797416844,-1.,2.07715226767559));
#21765=CARTESIAN_POINT('Ctrl Pts',(0.571816823242602,-1.,2.07261449292824));
#21766=CARTESIAN_POINT('Ctrl Pts',(0.567368421181087,-1.,2.06805732997334));
#21767=CARTESIAN_POINT('Ctrl Pts',(0.562955993082261,-1.,2.06348090160589));
#21768=CARTESIAN_POINT('Ctrl Pts',(0.558579940185151,-1.,2.05888537756462));
#21769=CARTESIAN_POINT('Ctrl Pts',(0.554240657463906,-1.,2.05427091604413));
#21770=CARTESIAN_POINT('Ctrl Pts',(0.549938525150295,-1.,2.04963761077958));
#21771=CARTESIAN_POINT('Ctrl Pts',(0.54567390381743,-1.,2.04498544714588));
#21772=CARTESIAN_POINT('Ctrl Pts',(0.541447120615659,-1.,2.04031422690527));
#21773=CARTESIAN_POINT('Ctrl Pts',(0.537258489833262,-1.,2.03562362954037));
#21774=CARTESIAN_POINT('Ctrl Pts',(0.533108355132976,-1.,2.03091336214426));
#21775=CARTESIAN_POINT('Ctrl Pts',(0.528997127241914,-1.,2.0261832908329));
#21776=CARTESIAN_POINT('Ctrl Pts',(0.524925318333476,-1.,2.02143356304698));
#21777=CARTESIAN_POINT('Ctrl Pts',(0.52089359039937,-1.,2.01666477917286));
#21778=CARTESIAN_POINT('Ctrl Pts',(0.516902681728687,-1.,2.01187773939242));
#21779=CARTESIAN_POINT('Ctrl Pts',(0.512953306961792,-1.,2.00707309946949));
#21780=CARTESIAN_POINT('Ctrl Pts',(0.509046069886157,-1.,2.00225107134734));
#21781=CARTESIAN_POINT('Ctrl Pts',(0.505181361323026,-1.,1.99741107463572));
#21782=CARTESIAN_POINT('Ctrl Pts',(0.501359287727146,-1.,1.99255149126155));
#21783=CARTESIAN_POINT('Ctrl Pts',(0.497579909545574,-1.,1.98767044752932));
#21784=CARTESIAN_POINT('Ctrl Pts',(0.493843476541494,-1.,1.98276658761821));
#21785=CARTESIAN_POINT('Ctrl Pts',(0.490150627860952,-1.,1.97783973019229));
#21786=CARTESIAN_POINT('Ctrl Pts',(0.486502692907658,-1.,1.97289186263272));
#21787=CARTESIAN_POINT('Ctrl Pts',(0.48290166212069,-1.,1.96792703422362));
#21788=CARTESIAN_POINT('Ctrl Pts',(0.479349583074855,-1.,1.96294933055943));
#21789=CARTESIAN_POINT('Ctrl Pts',(0.475848034683176,-1.,1.95796111148177));
#21790=CARTESIAN_POINT('Ctrl Pts',(0.472397672264072,-1.,1.95296148278133));
#21791=CARTESIAN_POINT('Ctrl Pts',(0.468997482913135,-1.,1.94794381136514));
#21792=CARTESIAN_POINT('Ctrl Pts',(0.46564546202603,-1.,1.9428979419619));
#21793=CARTESIAN_POINT('Ctrl Pts',(0.462340031009056,-1.,1.93781486640821));
#21794=CARTESIAN_POINT('Ctrl Pts',(0.459081234547926,-1.,1.93269066517934));
#21795=CARTESIAN_POINT('Ctrl Pts',(0.45587200517437,-1.,1.92753067150476));
#21796=CARTESIAN_POINT('Ctrl Pts',(0.452719478359432,-1.,1.92235380648502));
#21797=CARTESIAN_POINT('Ctrl Pts',(0.449632260106662,-1.,1.91718342555755));
#21798=CARTESIAN_POINT('Ctrl Pts',(0.446617343485711,-1.,1.9120369998112));
#21799=CARTESIAN_POINT('Ctrl Pts',(0.44367755684915,-1.,1.90691756144898));
#21800=CARTESIAN_POINT('Ctrl Pts',(0.440807833704038,-1.,1.90180124389086));
#21801=CARTESIAN_POINT('Ctrl Pts',(0.437995003948244,-1.,1.89663648956466));
#21802=CARTESIAN_POINT('Ctrl Pts',(0.435225660963383,-1.,1.89136993975504));
#21803=CARTESIAN_POINT('Ctrl Pts',(0.432493038548748,-1.,1.88596913666793));
#21804=CARTESIAN_POINT('Ctrl Pts',(0.429803062482344,-1.,1.88044229001832));
#21805=CARTESIAN_POINT('Ctrl Pts',(0.427183828519102,-1.,1.87486989291484));
#21806=CARTESIAN_POINT('Ctrl Pts',(0.424678177291358,-1.,1.86937803944323));
#21807=CARTESIAN_POINT('Ctrl Pts',(0.422327307418275,-1.,1.86408083334028));
#21808=CARTESIAN_POINT('Ctrl Pts',(0.420157287975619,-1.,1.85903281096686));
#21809=CARTESIAN_POINT('Ctrl Pts',(0.418164129143534,-1.,1.85417632856234));
#21810=CARTESIAN_POINT('Ctrl Pts',(0.416300022038864,-1.,1.84929312929882));
#21811=CARTESIAN_POINT('Ctrl Pts',(0.41448743825434,-1.,1.8440575707371));
#21812=CARTESIAN_POINT('Ctrl Pts',(0.412633125322161,-1.,1.83808953475839));
#21813=CARTESIAN_POINT('Ctrl Pts',(0.410641256301674,-1.,1.83100408895216));
#21814=CARTESIAN_POINT('Ctrl Pts',(0.408428948108533,-1.,1.8224702267854));
#21815=CARTESIAN_POINT('Ctrl Pts',(0.405933518411838,-1.,1.81223801813988));
#21816=CARTESIAN_POINT('Ctrl Pts',(0.403107976170441,-1.,1.80012077176221));
#21817=CARTESIAN_POINT('Ctrl Pts',(0.39991940378308,-1.,1.78598826347533));
#21818=CARTESIAN_POINT('Ctrl Pts',(0.39634619612042,-1.,1.7697556004756));
#21819=CARTESIAN_POINT('Ctrl Pts',(0.392375812294307,-1.,1.75137405313962));
#21820=CARTESIAN_POINT('Ctrl Pts',(0.388877023509191,-1.,1.7349317097561));
#21821=CARTESIAN_POINT('Ctrl Pts',(0.38607079032701,-1.,1.72162022246158));
#21822=CARTESIAN_POINT('Ctrl Pts',(0.384119047315541,-1.,1.71231062891958));
#21823=CARTESIAN_POINT('Ctrl Pts',(0.383122945602004,-1.,1.7075470150345));
#21824=CARTESIAN_POINT('',(0.163289472382896,-1.,1.74236521665491));
#21825=CARTESIAN_POINT('Origin',(0.,-1.,0.));
#21826=CARTESIAN_POINT('',(0.0694764450219578,-1.,2.19890268624765));
#21827=CARTESIAN_POINT('Ctrl Pts',(0.163289472382896,-1.,1.74236521665491));
#21828=CARTESIAN_POINT('Ctrl Pts',(0.163814161002002,-1.,1.7472034950333));
#21829=CARTESIAN_POINT('Ctrl Pts',(0.164834765707158,-1.,1.75666056638427));
#21830=CARTESIAN_POINT('Ctrl Pts',(0.1662793551464,-1.,1.77018771684844));
#21831=CARTESIAN_POINT('Ctrl Pts',(0.168032772805197,-1.,1.7869064998507));
#21832=CARTESIAN_POINT('Ctrl Pts',(0.169936923904608,-1.,1.80561530629706));
#21833=CARTESIAN_POINT('Ctrl Pts',(0.171554770204119,-1.,1.82215766811545));
#21834=CARTESIAN_POINT('Ctrl Pts',(0.1728894428919,-1.,1.83658380527692));
#21835=CARTESIAN_POINT('Ctrl Pts',(0.173946627587731,-1.,1.8489811319852));
#21836=CARTESIAN_POINT('Ctrl Pts',(0.17473525927603,-1.,1.85948367088837));
#21837=CARTESIAN_POINT('Ctrl Pts',(0.175268337590757,-1.,1.86828349694799));
#21838=CARTESIAN_POINT('Ctrl Pts',(0.175563480746485,-1.,1.87563767773588));
#21839=CARTESIAN_POINT('Ctrl Pts',(0.175644148889698,-1.,1.88188663145367));
#21840=CARTESIAN_POINT('Ctrl Pts',(0.175538155840648,-1.,1.88742606273259));
#21841=CARTESIAN_POINT('Ctrl Pts',(0.175274276190844,-1.,1.892646301985));
#21842=CARTESIAN_POINT('Ctrl Pts',(0.174879405091263,-1.,1.89788101117132));
#21843=CARTESIAN_POINT('Ctrl Pts',(0.174375518661085,-1.,1.90335253862834));
#21844=CARTESIAN_POINT('Ctrl Pts',(0.173776635257816,-1.,1.90911693975267));
#21845=CARTESIAN_POINT('Ctrl Pts',(0.173090695383496,-1.,1.91511429159527));
#21846=CARTESIAN_POINT('Ctrl Pts',(0.172321621259513,-1.,1.9212233439798));
#21847=CARTESIAN_POINT('Ctrl Pts',(0.171471191532988,-1.,1.92731093582036));
#21848=CARTESIAN_POINT('Ctrl Pts',(0.170541253116201,-1.,1.93329183155539));
#21849=CARTESIAN_POINT('Ctrl Pts',(0.16953490481749,-1.,1.93915639211581));
#21850=CARTESIAN_POINT('Ctrl Pts',(0.168455741607556,-1.,1.94493757756931));
#21851=CARTESIAN_POINT('Ctrl Pts',(0.167307501784475,-1.,1.95069027794294));
#21852=CARTESIAN_POINT('Ctrl Pts',(0.166093592002812,-1.,1.9564675971873));
#21853=CARTESIAN_POINT('Ctrl Pts',(0.164816568920269,-1.,1.96229379940136));
#21854=CARTESIAN_POINT('Ctrl Pts',(0.163478185457734,-1.,1.96816512677967));
#21855=CARTESIAN_POINT('Ctrl Pts',(0.162079693556288,-1.,1.97406280235188));
#21856=CARTESIAN_POINT('Ctrl Pts',(0.160622060784611,-1.,1.97996195437559));
#21857=CARTESIAN_POINT('Ctrl Pts',(0.159106226437299,-1.,1.98584238283292));
#21858=CARTESIAN_POINT('Ctrl Pts',(0.157533331459227,-1.,1.99169810931908));
#21859=CARTESIAN_POINT('Ctrl Pts',(0.155904629548783,-1.,1.99753284771497));
#21860=CARTESIAN_POINT('Ctrl Pts',(0.154221403049722,-1.,2.00335565310543));
#21861=CARTESIAN_POINT('Ctrl Pts',(0.152484883621449,-1.,2.00917680318424));
#21862=CARTESIAN_POINT('Ctrl Pts',(0.150696157673078,-1.,2.01500291940238));
#21863=CARTESIAN_POINT('Ctrl Pts',(0.148856124775337,-1.,2.02083464969894));
#21864=CARTESIAN_POINT('Ctrl Pts',(0.146965557332583,-1.,2.02666926182017));
#21865=CARTESIAN_POINT('Ctrl Pts',(0.145025140186057,-1.,2.03250223739942));
#21866=CARTESIAN_POINT('Ctrl Pts',(0.143035515058208,-1.,2.03832911025912));
#21867=CARTESIAN_POINT('Ctrl Pts',(0.140997332152546,-1.,2.04414757947916));
#21868=CARTESIAN_POINT('Ctrl Pts',(0.138911255368966,-1.,2.04995762001328));
#21869=CARTESIAN_POINT('Ctrl Pts',(0.136777941218043,-1.,2.05576044414264));
#21870=CARTESIAN_POINT('Ctrl Pts',(0.134598026192106,-1.,2.06155781517842));
#21871=CARTESIAN_POINT('Ctrl Pts',(0.13237211154771,-1.,2.06735123910326));
#21872=CARTESIAN_POINT('Ctrl Pts',(0.130100748328403,-1.,2.07314114713063));
#21873=CARTESIAN_POINT('Ctrl Pts',(0.12778444527612,-1.,2.07892715110987));
#21874=CARTESIAN_POINT('Ctrl Pts',(0.125423679412061,-1.,2.08470840653643));
#21875=CARTESIAN_POINT('Ctrl Pts',(0.123018905621083,-1.,2.09048392424825));
#21876=CARTESIAN_POINT('Ctrl Pts',(0.120570567965122,-1.,2.0962529286773));
#21877=CARTESIAN_POINT('Ctrl Pts',(0.118079107988355,-1.,2.102015121329));
#21878=CARTESIAN_POINT('Ctrl Pts',(0.115544957687926,-1.,2.10777050261309));
#21879=CARTESIAN_POINT('Ctrl Pts',(0.112968534419737,-1.,2.11351924490306));
#21880=CARTESIAN_POINT('Ctrl Pts',(0.110350236135025,-1.,2.11926155590865));
#21881=CARTESIAN_POINT('Ctrl Pts',(0.10769043523109,-1.,2.12499752307));
#21882=CARTESIAN_POINT('Ctrl Pts',(0.104989479152739,-1.,2.13072704887293));
#21883=CARTESIAN_POINT('Ctrl Pts',(0.1022477005561,-1.,2.13644992667165));
#21884=CARTESIAN_POINT('Ctrl Pts',(0.0994654261990913,-1.,2.14216588396025));
#21885=CARTESIAN_POINT('Ctrl Pts',(0.0966429852305456,-1.,2.14787463531795));
#21886=CARTESIAN_POINT('Ctrl Pts',(0.0937807218867641,-1.,2.1535759397817));
#21887=CARTESIAN_POINT('Ctrl Pts',(0.0908789888107263,-1.,2.15926961544516));
#21888=CARTESIAN_POINT('Ctrl Pts',(0.087938129138692,-1.,2.16495552645014));
#21889=CARTESIAN_POINT('Ctrl Pts',(0.084958462083537,-1.,2.17063357870952));
#21890=CARTESIAN_POINT('Ctrl Pts',(0.0819402680872763,-1.,2.176303712113));
#21891=CARTESIAN_POINT('Ctrl Pts',(0.078883772768524,-1.,2.18196589448887));
#21892=CARTESIAN_POINT('Ctrl Pts',(0.0757891465836145,-1.,2.1876201139953));
#21893=CARTESIAN_POINT('Ctrl Pts',(0.0732830357306722,-1.,2.19213712013662));
#21894=CARTESIAN_POINT('Ctrl Pts',(0.0713863779526151,-1.,2.19552129484002));
#21895=CARTESIAN_POINT('Ctrl Pts',(0.0701143536325487,-1.,2.19777582085423));
#21896=CARTESIAN_POINT('Ctrl Pts',(0.0694764450219578,-1.,2.19890268624765));
#21897=CARTESIAN_POINT('',(-0.0694764450219586,-1.,2.19890268624765));
#21898=CARTESIAN_POINT('',(0.0694764450219578,-1.,2.19890268624765));
#21899=CARTESIAN_POINT('',(-0.163289472382896,-1.,1.74236521665491));
#21900=CARTESIAN_POINT('Ctrl Pts',(-0.0694764450219586,-1.,2.19890268624765));
#21901=CARTESIAN_POINT('Ctrl Pts',(-0.0701143536324929,-1.,2.19777582085261));
#21902=CARTESIAN_POINT('Ctrl Pts',(-0.071386377952463,-1.,2.19552129483562));
#21903=CARTESIAN_POINT('Ctrl Pts',(-0.0732830357304279,-1.,2.19213712012956));
#21904=CARTESIAN_POINT('Ctrl Pts',(-0.0757891465833414,-1.,2.1876201139874));
#21905=CARTESIAN_POINT('Ctrl Pts',(-0.078883772768323,-1.,2.18196589448304));
#21906=CARTESIAN_POINT('Ctrl Pts',(-0.0819402680871942,-1.,2.1763037121106));
#21907=CARTESIAN_POINT('Ctrl Pts',(-0.0849584620835646,-1.,2.17063357871031));
#21908=CARTESIAN_POINT('Ctrl Pts',(-0.0879381291387825,-1.,2.16495552645275));
#21909=CARTESIAN_POINT('Ctrl Pts',(-0.0908789888108269,-1.,2.15926961544808));
#21910=CARTESIAN_POINT('Ctrl Pts',(-0.0937807218868348,-1.,2.15357593978377));
#21911=CARTESIAN_POINT('Ctrl Pts',(-0.0966429852305691,-1.,2.14787463531864));
#21912=CARTESIAN_POINT('Ctrl Pts',(-0.0994654261990745,-1.,2.14216588395974));
#21913=CARTESIAN_POINT('Ctrl Pts',(-0.102247700556064,-1.,2.13644992667052));
#21914=CARTESIAN_POINT('Ctrl Pts',(-0.104989479152703,-1.,2.1307270488718));
#21915=CARTESIAN_POINT('Ctrl Pts',(-0.107690435231068,-1.,2.12499752306927));
#21916=CARTESIAN_POINT('Ctrl Pts',(-0.11035023613502,-1.,2.11926155590849));
#21917=CARTESIAN_POINT('Ctrl Pts',(-0.112968534419746,-1.,2.11351924490335));
#21918=CARTESIAN_POINT('Ctrl Pts',(-0.115544957687941,-1.,2.10777050261359));
#21919=CARTESIAN_POINT('Ctrl Pts',(-0.118079107988368,-1.,2.10201512132945));
#21920=CARTESIAN_POINT('Ctrl Pts',(-0.120570567965129,-1.,2.09625292867756));
#21921=CARTESIAN_POINT('Ctrl Pts',(-0.123018905621083,-1.,2.09048392424826));
#21922=CARTESIAN_POINT('Ctrl Pts',(-0.125423679412058,-1.,2.08470840653628));
#21923=CARTESIAN_POINT('Ctrl Pts',(-0.127784445276116,-1.,2.07892715110967));
#21924=CARTESIAN_POINT('Ctrl Pts',(-0.130100748328401,-1.,2.07314114713047));
#21925=CARTESIAN_POINT('Ctrl Pts',(-0.13237211154771,-1.,2.06735123910319));
#21926=CARTESIAN_POINT('Ctrl Pts',(-0.134598026192107,-1.,2.06155781517844));
#21927=CARTESIAN_POINT('Ctrl Pts',(-0.136777941218044,-1.,2.0557604441427));
#21928=CARTESIAN_POINT('Ctrl Pts',(-0.138911255368966,-1.,2.04995762001333));
#21929=CARTESIAN_POINT('Ctrl Pts',(-0.140997332152546,-1.,2.04414757947919));
#21930=CARTESIAN_POINT('Ctrl Pts',(-0.143035515058208,-1.,2.03832911025913));
#21931=CARTESIAN_POINT('Ctrl Pts',(-0.145025140186058,-1.,2.03250223739941));
#21932=CARTESIAN_POINT('Ctrl Pts',(-0.146965557332586,-1.,2.02666926182017));
#21933=CARTESIAN_POINT('Ctrl Pts',(-0.148856124775343,-1.,2.02083464969897));
#21934=CARTESIAN_POINT('Ctrl Pts',(-0.150696157673084,-1.,2.01500291940243));
#21935=CARTESIAN_POINT('Ctrl Pts',(-0.152484883621452,-1.,2.00917680318426));
#21936=CARTESIAN_POINT('Ctrl Pts',(-0.154221403049719,-1.,2.00335565310539));
#21937=CARTESIAN_POINT('Ctrl Pts',(-0.155904629548775,-1.,1.99753284771487));
#21938=CARTESIAN_POINT('Ctrl Pts',(-0.157533331459215,-1.,1.99169810931893));
#21939=CARTESIAN_POINT('Ctrl Pts',(-0.159106226437289,-1.,1.98584238283279));
#21940=CARTESIAN_POINT('Ctrl Pts',(-0.16062206078461,-1.,1.97996195437557));
#21941=CARTESIAN_POINT('Ctrl Pts',(-0.162079693556302,-1.,1.97406280235204));
#21942=CARTESIAN_POINT('Ctrl Pts',(-0.16347818545776,-1.,1.96816512678));
#21943=CARTESIAN_POINT('Ctrl Pts',(-0.1648165689203,-1.,1.96229379940174));
#21944=CARTESIAN_POINT('Ctrl Pts',(-0.166093592002833,-1.,1.95646759718755));
#21945=CARTESIAN_POINT('Ctrl Pts',(-0.167307501784469,-1.,1.95069027794286));
#21946=CARTESIAN_POINT('Ctrl Pts',(-0.168455741607516,-1.,1.94493757756879));
#21947=CARTESIAN_POINT('Ctrl Pts',(-0.169534904817425,-1.,1.93915639211497));
#21948=CARTESIAN_POINT('Ctrl Pts',(-0.170541253116136,-1.,1.93329183155455));
#21949=CARTESIAN_POINT('Ctrl Pts',(-0.17147119153296,-1.,1.92731093582));
#21950=CARTESIAN_POINT('Ctrl Pts',(-0.172321621259557,-1.,1.92122334398034));
#21951=CARTESIAN_POINT('Ctrl Pts',(-0.173090695383619,-1.,1.91511429159681));
#21952=CARTESIAN_POINT('Ctrl Pts',(-0.173776635257984,-1.,1.90911693975475));
#21953=CARTESIAN_POINT('Ctrl Pts',(-0.174375518661222,-1.,1.90335253863003));
#21954=CARTESIAN_POINT('Ctrl Pts',(-0.174879405091277,-1.,1.89788101117148));
#21955=CARTESIAN_POINT('Ctrl Pts',(-0.175274276190664,-1.,1.89264630198279));
#21956=CARTESIAN_POINT('Ctrl Pts',(-0.175538155840286,-1.,1.88742606272818));
#21957=CARTESIAN_POINT('Ctrl Pts',(-0.175644148889271,-1.,1.88188663144846));
#21958=CARTESIAN_POINT('Ctrl Pts',(-0.175563480746206,-1.,1.87563767773249));
#21959=CARTESIAN_POINT('Ctrl Pts',(-0.175268337590901,-1.,1.86828349694972));
#21960=CARTESIAN_POINT('Ctrl Pts',(-0.174735259276856,-1.,1.85948367089838));
#21961=CARTESIAN_POINT('Ctrl Pts',(-0.173946627589401,-1.,1.84898113200543));
#21962=CARTESIAN_POINT('Ctrl Pts',(-0.17288944289442,-1.,1.83658380530747));
#21963=CARTESIAN_POINT('Ctrl Pts',(-0.171554770207306,-1.,1.82215766815414));
#21964=CARTESIAN_POINT('Ctrl Pts',(-0.169936923908078,-1.,1.80561530633924));
#21965=CARTESIAN_POINT('Ctrl Pts',(-0.16803277280837,-1.,1.78690649988931));
#21966=CARTESIAN_POINT('Ctrl Pts',(-0.166279355148738,-1.,1.77018771687692));
#21967=CARTESIAN_POINT('Ctrl Pts',(-0.164834765708484,-1.,1.75666056640041));
#21968=CARTESIAN_POINT('Ctrl Pts',(-0.163814161002474,-1.,1.74720349503904));
#21969=CARTESIAN_POINT('Ctrl Pts',(-0.163289472382896,-1.,1.74236521665491));
#21970=CARTESIAN_POINT('',(-0.383122945602004,-1.,1.7075470150345));
#21971=CARTESIAN_POINT('Origin',(0.,-1.,0.));
#21972=CARTESIAN_POINT('',(-0.61342227326009,-1.,2.11275013067528));
#21973=CARTESIAN_POINT('Ctrl Pts',(-0.383122945602004,-1.,1.7075470150345));
#21974=CARTESIAN_POINT('Ctrl Pts',(-0.384119047314215,-1.,1.71231062891398));
#21975=CARTESIAN_POINT('Ctrl Pts',(-0.386070790323281,-1.,1.72162022244582));
#21976=CARTESIAN_POINT('Ctrl Pts',(-0.388877023502615,-1.,1.73493170972829));
#21977=CARTESIAN_POINT('Ctrl Pts',(-0.392375812285395,-1.,1.75137405310193));
#21978=CARTESIAN_POINT('Ctrl Pts',(-0.396346196110688,-1.,1.76975560043442));
#21979=CARTESIAN_POINT('Ctrl Pts',(-0.399919403774155,-1.,1.78598826343754));
#21980=CARTESIAN_POINT('Ctrl Pts',(-0.403107976163396,-1.,1.80012077173238));
#21981=CARTESIAN_POINT('Ctrl Pts',(-0.405933518407175,-1.,1.81223801812013));
#21982=CARTESIAN_POINT('Ctrl Pts',(-0.408428948106227,-1.,1.82247022677562));
#21983=CARTESIAN_POINT('Ctrl Pts',(-0.410641256301276,-1.,1.83100408895047));
#21984=CARTESIAN_POINT('Ctrl Pts',(-0.412633125322945,-1.,1.8380895347617));
#21985=CARTESIAN_POINT('Ctrl Pts',(-0.414487438255542,-1.,1.84405757074218));
#21986=CARTESIAN_POINT('Ctrl Pts',(-0.416300022039885,-1.,1.84929312930314));
#21987=CARTESIAN_POINT('Ctrl Pts',(-0.418164129144045,-1.,1.8541763285645));
#21988=CARTESIAN_POINT('Ctrl Pts',(-0.420157287975583,-1.,1.8590328109667));
#21989=CARTESIAN_POINT('Ctrl Pts',(-0.422327307417885,-1.,1.86408083333863));
#21990=CARTESIAN_POINT('Ctrl Pts',(-0.424678177290876,-1.,1.8693780394412));
#21991=CARTESIAN_POINT('Ctrl Pts',(-0.427183828518743,-1.,1.87486989291333));
#21992=CARTESIAN_POINT('Ctrl Pts',(-0.429803062482217,-1.,1.88044229001778));
#21993=CARTESIAN_POINT('Ctrl Pts',(-0.432493038548833,-1.,1.88596913666828));
#21994=CARTESIAN_POINT('Ctrl Pts',(-0.43522566096358,-1.,1.89136993975585));
#21995=CARTESIAN_POINT('Ctrl Pts',(-0.437995003948443,-1.,1.89663648956549));
#21996=CARTESIAN_POINT('Ctrl Pts',(-0.440807833704161,-1.,1.90180124389137));
#21997=CARTESIAN_POINT('Ctrl Pts',(-0.44367755684917,-1.,1.90691756144906));
#21998=CARTESIAN_POINT('Ctrl Pts',(-0.446617343485651,-1.,1.91203699981095));
#21999=CARTESIAN_POINT('Ctrl Pts',(-0.449632260106572,-1.,1.91718342555717));
#22000=CARTESIAN_POINT('Ctrl Pts',(-0.452719478359356,-1.,1.9223538064847));
#22001=CARTESIAN_POINT('Ctrl Pts',(-0.455872005174335,-1.,1.92753067150461));
#22002=CARTESIAN_POINT('Ctrl Pts',(-0.459081234547931,-1.,1.93269066517936));
#22003=CARTESIAN_POINT('Ctrl Pts',(-0.462340031009087,-1.,1.93781486640834));
#22004=CARTESIAN_POINT('Ctrl Pts',(-0.465645462026065,-1.,1.94289794196205));
#22005=CARTESIAN_POINT('Ctrl Pts',(-0.468997482913158,-1.,1.94794381136524));
#22006=CARTESIAN_POINT('Ctrl Pts',(-0.47239767226408,-1.,1.95296148278136));
#22007=CARTESIAN_POINT('Ctrl Pts',(-0.475848034683172,-1.,1.95796111148175));
#22008=CARTESIAN_POINT('Ctrl Pts',(-0.479349583074846,-1.,1.96294933055938));
#22009=CARTESIAN_POINT('Ctrl Pts',(-0.482901662120687,-1.,1.96792703422358));
#22010=CARTESIAN_POINT('Ctrl Pts',(-0.486502692907661,-1.,1.97289186263272));
#22011=CARTESIAN_POINT('Ctrl Pts',(-0.490150627860955,-1.,1.97783973019229));
#22012=CARTESIAN_POINT('Ctrl Pts',(-0.493843476541492,-1.,1.9827665876182));
#22013=CARTESIAN_POINT('Ctrl Pts',(-0.497579909545564,-1.,1.98767044752929));
#22014=CARTESIAN_POINT('Ctrl Pts',(-0.501359287727129,-1.,1.9925514912615));
#22015=CARTESIAN_POINT('Ctrl Pts',(-0.505181361323011,-1.,1.99741107463567));
#22016=CARTESIAN_POINT('Ctrl Pts',(-0.509046069886152,-1.,2.00225107134733));
#22017=CARTESIAN_POINT('Ctrl Pts',(-0.512953306961814,-1.,2.00707309946955));
#22018=CARTESIAN_POINT('Ctrl Pts',(-0.516902681728733,-1.,2.01187773939257));
#22019=CARTESIAN_POINT('Ctrl Pts',(-0.520893590399428,-1.,2.01666477917305));
#22020=CARTESIAN_POINT('Ctrl Pts',(-0.524925318333518,-1.,2.02143356304712));
#22021=CARTESIAN_POINT('Ctrl Pts',(-0.528997127241911,-1.,2.02618329083289));
#22022=CARTESIAN_POINT('Ctrl Pts',(-0.533108355132905,-1.,2.03091336214401));
#22023=CARTESIAN_POINT('Ctrl Pts',(-0.537258489833134,-1.,2.03562362953993));
#22024=CARTESIAN_POINT('Ctrl Pts',(-0.54144712061552,-1.,2.0403142269048));
#22025=CARTESIAN_POINT('Ctrl Pts',(-0.545673903817348,-1.,2.0449854471456));
#22026=CARTESIAN_POINT('Ctrl Pts',(-0.549938525150342,-1.,2.04963761077974));
#22027=CARTESIAN_POINT('Ctrl Pts',(-0.55424065746411,-1.,2.05427091604482));
#22028=CARTESIAN_POINT('Ctrl Pts',(-0.558579940185467,-1.,2.05888537756571));
#22029=CARTESIAN_POINT('Ctrl Pts',(-0.562955993082574,-1.,2.06348090160697));
#22030=CARTESIAN_POINT('Ctrl Pts',(-0.567368421181229,-1.,2.06805732997383));
#22031=CARTESIAN_POINT('Ctrl Pts',(-0.571816823242411,-1.,2.07261449292757));
#22032=CARTESIAN_POINT('Ctrl Pts',(-0.576300797416275,-1.,2.07715226767361));
#22033=CARTESIAN_POINT('Ctrl Pts',(-0.580819952107257,-1.,2.08167059018138));
#22034=CARTESIAN_POINT('Ctrl Pts',(-0.585373918990895,-1.,2.086169437277));
#22035=CARTESIAN_POINT('Ctrl Pts',(-0.589962365403189,-1.,2.09064881812053));
#22036=CARTESIAN_POINT('Ctrl Pts',(-0.594585006052824,-1.,2.09510876220501));
#22037=CARTESIAN_POINT('Ctrl Pts',(-0.599241616422144,-1.,2.09954930865331));
#22038=CARTESIAN_POINT('Ctrl Pts',(-0.603932030738212,-1.,2.10397049887709));
#22039=CARTESIAN_POINT('Ctrl Pts',(-0.607711315456826,-1.,2.10749199615859));
#22040=CARTESIAN_POINT('Ctrl Pts',(-0.610560911691113,-1.,2.11012443807661));
#22041=CARTESIAN_POINT('Ctrl Pts',(-0.61246736556225,-1.,2.11187554260142));
#22042=CARTESIAN_POINT('Ctrl Pts',(-0.61342227326009,-1.,2.11275013067528));
#22043=CARTESIAN_POINT('',(-0.745574324794401,-1.,2.0698113262342));
#22044=CARTESIAN_POINT('',(-0.61342227326009,-1.,2.11275013067528));
#22045=CARTESIAN_POINT('',(-0.693717979106306,-1.,1.60662857109684));
#22046=CARTESIAN_POINT('Ctrl Pts',(-0.745574324794401,-1.,2.0698113262342));
#22047=CARTESIAN_POINT('Ctrl Pts',(-0.74583279137781,-1.,2.06854248895575));
#22048=CARTESIAN_POINT('Ctrl Pts',(-0.746345871542696,-1.,2.06600523016401));
#22049=CARTESIAN_POINT('Ctrl Pts',(-0.747103932785504,-1.,2.06220058927162));
#22050=CARTESIAN_POINT('Ctrl Pts',(-0.748091554181101,-1.,2.05713023030263));
#22051=CARTESIAN_POINT('Ctrl Pts',(-0.749287468663053,-1.,2.05079645591606));
#22052=CARTESIAN_POINT('Ctrl Pts',(-0.750444657874758,-1.,2.04446689147754));
#22053=CARTESIAN_POINT('Ctrl Pts',(-0.751562963361384,-1.,2.03814160092173));
#22054=CARTESIAN_POINT('Ctrl Pts',(-0.752642180488104,-1.,2.03182068456467));
#22055=CARTESIAN_POINT('Ctrl Pts',(-0.753682061113766,-1.,2.02550428623587));
#22056=CARTESIAN_POINT('Ctrl Pts',(-0.75468233072352,-1.,2.01919259406003));
#22057=CARTESIAN_POINT('Ctrl Pts',(-0.7556427049581,-1.,2.01288584328149));
#22058=CARTESIAN_POINT('Ctrl Pts',(-0.756562904646496,-1.,2.00658431587682));
#22059=CARTESIAN_POINT('Ctrl Pts',(-0.757442676862341,-1.,2.00028834739072));
#22060=CARTESIAN_POINT('Ctrl Pts',(-0.758281796766377,-1.,1.9939983109871));
#22061=CARTESIAN_POINT('Ctrl Pts',(-0.759080037802243,-1.,1.98771456680806));
#22062=CARTESIAN_POINT('Ctrl Pts',(-0.759837147452135,-1.,1.98143741418156));
#22063=CARTESIAN_POINT('Ctrl Pts',(-0.760552825409855,-1.,1.97516705321521));
#22064=CARTESIAN_POINT('Ctrl Pts',(-0.761226690483986,-1.,1.96890351582545));
#22065=CARTESIAN_POINT('Ctrl Pts',(-0.761858300014575,-1.,1.96264672744229));
#22066=CARTESIAN_POINT('Ctrl Pts',(-0.762447203806263,-1.,1.95639665309893));
#22067=CARTESIAN_POINT('Ctrl Pts',(-0.762992990878774,-1.,1.95015342590025));
#22068=CARTESIAN_POINT('Ctrl Pts',(-0.76349533353858,-1.,1.94391746617626));
#22069=CARTESIAN_POINT('Ctrl Pts',(-0.763954049121393,-1.,1.93768964875867));
#22070=CARTESIAN_POINT('Ctrl Pts',(-0.764369010673889,-1.,1.93147105496367));
#22071=CARTESIAN_POINT('Ctrl Pts',(-0.764740025488189,-1.,1.92526263537041));
#22072=CARTESIAN_POINT('Ctrl Pts',(-0.765066729667095,-1.,1.91906491634197));
#22073=CARTESIAN_POINT('Ctrl Pts',(-0.765348465884739,-1.,1.91287765805174));
#22074=CARTESIAN_POINT('Ctrl Pts',(-0.765584196937936,-1.,1.90669961402362));
#22075=CARTESIAN_POINT('Ctrl Pts',(-0.765772772593395,-1.,1.90052930393599));
#22076=CARTESIAN_POINT('Ctrl Pts',(-0.765913193856979,-1.,1.89436577771389));
#22077=CARTESIAN_POINT('Ctrl Pts',(-0.76600483706209,-1.,1.88820926433409));
#22078=CARTESIAN_POINT('Ctrl Pts',(-0.766047794851869,-1.,1.88206215302561));
#22079=CARTESIAN_POINT('Ctrl Pts',(-0.766042837036759,-1.,1.87592888967886));
#22080=CARTESIAN_POINT('Ctrl Pts',(-0.765990708546111,-1.,1.86981398314345));
#22081=CARTESIAN_POINT('Ctrl Pts',(-0.765891519092557,-1.,1.86372027063314));
#22082=CARTESIAN_POINT('Ctrl Pts',(-0.765744212909305,-1.,1.85764741390391));
#22083=CARTESIAN_POINT('Ctrl Pts',(-0.765545710619023,-1.,1.85158945130054));
#22084=CARTESIAN_POINT('Ctrl Pts',(-0.765291664861971,-1.,1.8455369887591));
#22085=CARTESIAN_POINT('Ctrl Pts',(-0.764978057881687,-1.,1.83948181064823));
#22086=CARTESIAN_POINT('Ctrl Pts',(-0.764602549687845,-1.,1.8334207722714));
#22087=CARTESIAN_POINT('Ctrl Pts',(-0.764165902606055,-1.,1.8273599120008));
#22088=CARTESIAN_POINT('Ctrl Pts',(-0.763673465462854,-1.,1.82131873145297));
#22089=CARTESIAN_POINT('Ctrl Pts',(-0.763132003836783,-1.,1.81532118405566));
#22090=CARTESIAN_POINT('Ctrl Pts',(-0.762546129464036,-1.,1.80938551463989));
#22091=CARTESIAN_POINT('Ctrl Pts',(-0.761915336443516,-1.,1.80351583877334));
#22092=CARTESIAN_POINT('Ctrl Pts',(-0.761229695230359,-1.,1.79768986997735));
#22093=CARTESIAN_POINT('Ctrl Pts',(-0.760469555880425,-1.,1.79185815610802));
#22094=CARTESIAN_POINT('Ctrl Pts',(-0.759614401109868,-1.,1.78596964884526));
#22095=CARTESIAN_POINT('Ctrl Pts',(-0.75865062667738,-1.,1.77999411220912));
#22096=CARTESIAN_POINT('Ctrl Pts',(-0.757578264077238,-1.,1.77394167108342));
#22097=CARTESIAN_POINT('Ctrl Pts',(-0.756421896028403,-1.,1.76789396003141));
#22098=CARTESIAN_POINT('Ctrl Pts',(-0.755220979975262,-1.,1.7619781724032));
#22099=CARTESIAN_POINT('Ctrl Pts',(-0.75400925402848,-1.,1.75631083600175));
#22100=CARTESIAN_POINT('Ctrl Pts',(-0.752797683531377,-1.,1.75095139468809));
#22101=CARTESIAN_POINT('Ctrl Pts',(-0.751555614163629,-1.,1.74585086852298));
#22102=CARTESIAN_POINT('Ctrl Pts',(-0.75019343597954,-1.,1.74080458266705));
#22103=CARTESIAN_POINT('Ctrl Pts',(-0.748582462954855,-1.,1.73550351679848));
#22104=CARTESIAN_POINT('Ctrl Pts',(-0.746574710096436,-1.,1.72958533647399));
#22105=CARTESIAN_POINT('Ctrl Pts',(-0.744021445433764,-1.,1.7226822991693));
#22106=CARTESIAN_POINT('Ctrl Pts',(-0.740795162032088,-1.,1.71447789751927));
#22107=CARTESIAN_POINT('Ctrl Pts',(-0.736799665724771,-1.,1.70473309006121));
#22108=CARTESIAN_POINT('Ctrl Pts',(-0.731963238697195,-1.,1.69326921975743));
#22109=CARTESIAN_POINT('Ctrl Pts',(-0.726235967997433,-1.,1.67996158455503));
#22110=CARTESIAN_POINT('Ctrl Pts',(-0.719585433804282,-1.,1.6647288055568));
#22111=CARTESIAN_POINT('Ctrl Pts',(-0.711993139355394,-1.,1.64752408832016));
#22112=CARTESIAN_POINT('Ctrl Pts',(-0.705159151988319,-1.,1.63216541664676));
#22113=CARTESIAN_POINT('Ctrl Pts',(-0.699605146405088,-1.,1.61974673472612));
#22114=CARTESIAN_POINT('Ctrl Pts',(-0.695712097881194,-1.,1.61106790958151));
#22115=CARTESIAN_POINT('Ctrl Pts',(-0.693717979106306,-1.,1.60662857109684));
#22116=CARTESIAN_POINT('',(-0.892032620296855,-1.,1.5055822144029));
#22117=CARTESIAN_POINT('Origin',(0.,-1.,0.));
#22118=CARTESIAN_POINT('',(-1.23627494547115,-1.,1.81978687191668));
#22119=CARTESIAN_POINT('Ctrl Pts',(-0.892032620296855,-1.,1.5055822144029));
#22120=CARTESIAN_POINT('Ctrl Pts',(-0.894452006964543,-1.,1.50980486806688));
#22121=CARTESIAN_POINT('Ctrl Pts',(-0.899185047483511,-1.,1.51805569590094));
#22122=CARTESIAN_POINT('Ctrl Pts',(-0.905967409625651,-1.,1.52984849887993));
#22123=CARTESIAN_POINT('Ctrl Pts',(-0.914375919026456,-1.,1.54440491149498));
#22124=CARTESIAN_POINT('Ctrl Pts',(-0.923832188944341,-1.,1.56065988578893));
#22125=CARTESIAN_POINT('Ctrl Pts',(-0.932246680108685,-1.,1.57499388382243));
#22126=CARTESIAN_POINT('Ctrl Pts',(-0.939646377893399,-1.,1.58744937487176));
#22127=CARTESIAN_POINT('Ctrl Pts',(-0.946078063315257,-1.,1.59810042043673));
#22128=CARTESIAN_POINT('Ctrl Pts',(-0.951613284356035,-1.,1.60706069896936));
#22129=CARTESIAN_POINT('Ctrl Pts',(-0.956354422920671,-1.,1.61449324337085));
#22130=CARTESIAN_POINT('Ctrl Pts',(-0.960438326101729,-1.,1.62061638140221));
#22131=CARTESIAN_POINT('Ctrl Pts',(-0.964046107040536,-1.,1.62571930670187));
#22132=CARTESIAN_POINT('Ctrl Pts',(-0.967387853230345,-1.,1.63013849959461));
#22133=CARTESIAN_POINT('Ctrl Pts',(-0.970669715997509,-1.,1.63420665729798));
#22134=CARTESIAN_POINT('Ctrl Pts',(-0.974066058287418,-1.,1.63820952658144));
#22135=CARTESIAN_POINT('Ctrl Pts',(-0.977689794119416,-1.,1.64233990826687));
#22136=CARTESIAN_POINT('Ctrl Pts',(-0.981562530939489,-1.,1.64665139190656));
#22137=CARTESIAN_POINT('Ctrl Pts',(-0.985642622920821,-1.,1.65110016612638));
#22138=CARTESIAN_POINT('Ctrl Pts',(-0.989855627854165,-1.,1.65559044289699));
#22139=CARTESIAN_POINT('Ctrl Pts',(-0.994121836661306,-1.,1.66001553809947));
#22140=CARTESIAN_POINT('Ctrl Pts',(-0.998389654952758,-1.,1.66430758030376));
#22141=CARTESIAN_POINT('Ctrl Pts',(-1.00265091003727,-1.,1.66846059277303));
#22142=CARTESIAN_POINT('Ctrl Pts',(-1.00692206696414,-1.,1.67250335383293));
#22143=CARTESIAN_POINT('Ctrl Pts',(-1.01123236493511,-1.,1.67648246776464));
#22144=CARTESIAN_POINT('Ctrl Pts',(-1.01561026162773,-1.,1.68044289894798));
#22145=CARTESIAN_POINT('Ctrl Pts',(-1.02006795074201,-1.,1.68440578021706));
#22146=CARTESIAN_POINT('Ctrl Pts',(-1.02460180535255,-1.,1.68836910178447));
#22147=CARTESIAN_POINT('Ctrl Pts',(-1.02919977579147,-1.,1.69231840863458));
#22148=CARTESIAN_POINT('Ctrl Pts',(-1.03384646003588,-1.,1.69623414782771));
#22149=CARTESIAN_POINT('Ctrl Pts',(-1.03852922490789,-1.,1.70010052930962));
#22150=CARTESIAN_POINT('Ctrl Pts',(-1.04324363334554,-1.,1.70391338707982));
#22151=CARTESIAN_POINT('Ctrl Pts',(-1.04799085404995,-1.,1.70767646263649));
#22152=CARTESIAN_POINT('Ctrl Pts',(-1.05277517202855,-1.,1.71139783543989));
#22153=CARTESIAN_POINT('Ctrl Pts',(-1.05760163192479,-1.,1.7150865442702));
#22154=CARTESIAN_POINT('Ctrl Pts',(-1.06247324680647,-1.,1.71874858456904));
#22155=CARTESIAN_POINT('Ctrl Pts',(-1.06738966975462,-1.,1.72238500928453));
#22156=CARTESIAN_POINT('Ctrl Pts',(-1.07234866990252,-1.,1.72599406198488));
#22157=CARTESIAN_POINT('Ctrl Pts',(-1.0773470373727,-1.,1.72957248977424));
#22158=CARTESIAN_POINT('Ctrl Pts',(-1.08238162784749,-1.,1.73311705663407));
#22159=CARTESIAN_POINT('Ctrl Pts',(-1.08745056285427,-1.,1.73662628326091));
#22160=CARTESIAN_POINT('Ctrl Pts',(-1.09255329056493,-1.,1.74010053962247));
#22161=CARTESIAN_POINT('Ctrl Pts',(-1.09768999241225,-1.,1.74354119236208));
#22162=CARTESIAN_POINT('Ctrl Pts',(-1.10286118991143,-1.,1.74695004214923));
#22163=CARTESIAN_POINT('Ctrl Pts',(-1.10806728183007,-1.,1.7503286607592));
#22164=CARTESIAN_POINT('Ctrl Pts',(-1.11330807582551,-1.,1.7536777209463));
#22165=CARTESIAN_POINT('Ctrl Pts',(-1.11858293216763,-1.,1.75699720772105));
#22166=CARTESIAN_POINT('Ctrl Pts',(-1.12389096855086,-1.,1.76028671825096));
#22167=CARTESIAN_POINT('Ctrl Pts',(-1.12923123555075,-1.,1.7635457196617));
#22168=CARTESIAN_POINT('Ctrl Pts',(-1.1346029180462,-1.,1.76677384551862));
#22169=CARTESIAN_POINT('Ctrl Pts',(-1.14000548336975,-1.,1.76997111386769));
#22170=CARTESIAN_POINT('Ctrl Pts',(-1.1454385822692,-1.,1.77313777896194));
#22171=CARTESIAN_POINT('Ctrl Pts',(-1.15090197841515,-1.,1.7762742255701));
#22172=CARTESIAN_POINT('Ctrl Pts',(-1.15639547194698,-1.,1.77938085564275));
#22173=CARTESIAN_POINT('Ctrl Pts',(-1.16191881298499,-1.,1.78245795881009));
#22174=CARTESIAN_POINT('Ctrl Pts',(-1.16747166312303,-1.,1.78550566040443));
#22175=CARTESIAN_POINT('Ctrl Pts',(-1.17305363177328,-1.,1.78852398877616));
#22176=CARTESIAN_POINT('Ctrl Pts',(-1.17866429440809,-1.,1.79151291552689));
#22177=CARTESIAN_POINT('Ctrl Pts',(-1.18430321697432,-1.,1.79447240321515));
#22178=CARTESIAN_POINT('Ctrl Pts',(-1.18996997934445,-1.,1.79740245923478));
#22179=CARTESIAN_POINT('Ctrl Pts',(-1.19566418930242,-1.,1.80030314369879));
#22180=CARTESIAN_POINT('Ctrl Pts',(-1.20138548938974,-1.,1.80317454838603));
#22181=CARTESIAN_POINT('Ctrl Pts',(-1.20713356605475,-1.,1.80601678480707));
#22182=CARTESIAN_POINT('Ctrl Pts',(-1.21290815708314,-1.,1.80882996917129));
#22183=CARTESIAN_POINT('Ctrl Pts',(-1.21870906103557,-1.,1.81161420806656));
#22184=CARTESIAN_POINT('Ctrl Pts',(-1.2245361330495,-1.,1.81436959210434));
#22185=CARTESIAN_POINT('Ctrl Pts',(-1.2292186489137,-1.,1.8165508718364));
#22186=CARTESIAN_POINT('Ctrl Pts',(-1.2327422452705,-1.,1.81817389921279));
#22187=CARTESIAN_POINT('Ctrl Pts',(-1.23509651170476,-1.,1.81925017193666));
#22188=CARTESIAN_POINT('Ctrl Pts',(-1.23627494547115,-1.,1.81978687191668));
#22189=CARTESIAN_POINT('',(-1.34869019493419,-1.,1.73811241238545));
#22190=CARTESIAN_POINT('',(-1.23627494547115,-1.,1.81978687191668));
#22191=CARTESIAN_POINT('',(-1.15624053661742,-1.,1.31362392696032));
#22192=CARTESIAN_POINT('Ctrl Pts',(-1.34869019493419,-1.,1.73811241238545));
#22193=CARTESIAN_POINT('Ctrl Pts',(-1.34854391898045,-1.,1.73682580585691));
#22194=CARTESIAN_POINT('Ctrl Pts',(-1.34824783112887,-1.,1.73425417885907));
#22195=CARTESIAN_POINT('Ctrl Pts',(-1.34779309152035,-1.,1.7304014965394));
#22196=CARTESIAN_POINT('Ctrl Pts',(-1.34716554819527,-1.,1.72527410680674));
#22197=CARTESIAN_POINT('Ctrl Pts',(-1.34634568653227,-1.,1.7188807715049));
#22198=CARTESIAN_POINT('Ctrl Pts',(-1.34549029589416,-1.,1.71250340686822));
#22199=CARTESIAN_POINT('Ctrl Pts',(-1.34459924533831,-1.,1.70614212266738));
#22200=CARTESIAN_POINT('Ctrl Pts',(-1.34367237124483,-1.,1.69979707754427));
#22201=CARTESIAN_POINT('Ctrl Pts',(-1.34270948206319,-1.,1.6934684849687));
#22202=CARTESIAN_POINT('Ctrl Pts',(-1.341710374848,-1.,1.68715660868764));
#22203=CARTESIAN_POINT('Ctrl Pts',(-1.34067485185203,-1.,1.68086176030362));
#22204=CARTESIAN_POINT('Ctrl Pts',(-1.3396027347034,-1.,1.67458429426086));
#22205=CARTESIAN_POINT('Ctrl Pts',(-1.33849388654388,-1.,1.66832460783989));
#22206=CARTESIAN_POINT('Ctrl Pts',(-1.33734820885262,-1.,1.66208312541983));
#22207=CARTESIAN_POINT('Ctrl Pts',(-1.33616559745172,-1.,1.65586025952593));
#22208=CARTESIAN_POINT('Ctrl Pts',(-1.33494590467993,-1.,1.6496563728683));
#22209=CARTESIAN_POINT('Ctrl Pts',(-1.33368890676572,-1.,1.6434717485603));
#22210=CARTESIAN_POINT('Ctrl Pts',(-1.33239425103724,-1.,1.63730653475089));
#22211=CARTESIAN_POINT('Ctrl Pts',(-1.33106149345645,-1.,1.63116079730923));
#22212=CARTESIAN_POINT('Ctrl Pts',(-1.3296901950568,-1.,1.62503464209797));
#22213=CARTESIAN_POINT('Ctrl Pts',(-1.32828000610449,-1.,1.61892832270724));
#22214=CARTESIAN_POINT('Ctrl Pts',(-1.32683074483356,-1.,1.6128423401575));
#22215=CARTESIAN_POINT('Ctrl Pts',(-1.32534250785782,-1.,1.60677758290954));
#22216=CARTESIAN_POINT('Ctrl Pts',(-1.32381550858256,-1.,1.60073511858687));
#22217=CARTESIAN_POINT('Ctrl Pts',(-1.32224985747682,-1.,1.59471591079403));
#22218=CARTESIAN_POINT('Ctrl Pts',(-1.32064537110892,-1.,1.58872057258245));
#22219=CARTESIAN_POINT('Ctrl Pts',(-1.31900135021432,-1.,1.58274907898834));
#22220=CARTESIAN_POINT('Ctrl Pts',(-1.31731642317187,-1.,1.5768005650559));
#22221=CARTESIAN_POINT('Ctrl Pts',(-1.31558903860016,-1.,1.57087397835723));
#22222=CARTESIAN_POINT('Ctrl Pts',(-1.31381795281002,-1.,1.56496872402353));
#22223=CARTESIAN_POINT('Ctrl Pts',(-1.31200264341696,-1.,1.55908521254821));
#22224=CARTESIAN_POINT('Ctrl Pts',(-1.31014393684222,-1.,1.55322568759481));
#22225=CARTESIAN_POINT('Ctrl Pts',(-1.30824393907473,-1.,1.54739413957185));
#22226=CARTESIAN_POINT('Ctrl Pts',(-1.30630475189556,-1.,1.54159462645432));
#22227=CARTESIAN_POINT('Ctrl Pts',(-1.30432735639489,-1.,1.53582981268977));
#22228=CARTESIAN_POINT('Ctrl Pts',(-1.30231064395568,-1.,1.53009970283891));
#22229=CARTESIAN_POINT('Ctrl Pts',(-1.30024984366328,-1.,1.52439957861062));
#22230=CARTESIAN_POINT('Ctrl Pts',(-1.29813791800747,-1.,1.51872184912724));
#22231=CARTESIAN_POINT('Ctrl Pts',(-1.29596850710509,-1.,1.51305994241402));
#22232=CARTESIAN_POINT('Ctrl Pts',(-1.29373841372842,-1.,1.50741159078365));
#22233=CARTESIAN_POINT('Ctrl Pts',(-1.29145022885181,-1.,1.50178230149776));
#22234=CARTESIAN_POINT('Ctrl Pts',(-1.28911506584254,-1.,1.49618896881754));
#22235=CARTESIAN_POINT('Ctrl Pts',(-1.2867467611644,-1.,1.4906522831278));
#22236=CARTESIAN_POINT('Ctrl Pts',(-1.28435533880201,-1.,1.4851881711891));
#22237=CARTESIAN_POINT('Ctrl Pts',(-1.28194158939517,-1.,1.47980070347095));
#22238=CARTESIAN_POINT('Ctrl Pts',(-1.2794891824849,-1.,1.4744717526707));
#22239=CARTESIAN_POINT('Ctrl Pts',(-1.27696414831089,-1.,1.46916035917133));
#22240=CARTESIAN_POINT('Ctrl Pts',(-1.27433119897822,-1.,1.46382431332476));
#22241=CARTESIAN_POINT('Ctrl Pts',(-1.27156805265289,-1.,1.45843906294697));
#22242=CARTESIAN_POINT('Ctrl Pts',(-1.2686778680489,-1.,1.45301422764247));
#22243=CARTESIAN_POINT('Ctrl Pts',(-1.26570925118868,-1.,1.44761985001662));
#22244=CARTESIAN_POINT('Ctrl Pts',(-1.26273903323859,-1.,1.44236470511303));
#22245=CARTESIAN_POINT('Ctrl Pts',(-1.25983531012005,-1.,1.43734919180848));
#22246=CARTESIAN_POINT('Ctrl Pts',(-1.25702687965755,-1.,1.43262645609691));
#22247=CARTESIAN_POINT('Ctrl Pts',(-1.25426945222639,-1.,1.42815938799387));
#22248=CARTESIAN_POINT('Ctrl Pts',(-1.2514145557001,-1.,1.42378102115575));
#22249=CARTESIAN_POINT('Ctrl Pts',(-1.24824430986571,-1.,1.41923722596025));
#22250=CARTESIAN_POINT('Ctrl Pts',(-1.24450600513056,-1.,1.41422913175179));
#22251=CARTESIAN_POINT('Ctrl Pts',(-1.23994455029534,-1.,1.40845295531283));
#22252=CARTESIAN_POINT('Ctrl Pts',(-1.23434087290423,-1.,1.40164708206106));
#22253=CARTESIAN_POINT('Ctrl Pts',(-1.22752961899387,-1.,1.39361389568796));
#22254=CARTESIAN_POINT('Ctrl Pts',(-1.21938737280852,-1.,1.38420564527715));
#22255=CARTESIAN_POINT('Ctrl Pts',(-1.20982812925645,-1.,1.37331915607905));
#22256=CARTESIAN_POINT('Ctrl Pts',(-1.1987959077932,-1.,1.36088705043885));
#22257=CARTESIAN_POINT('Ctrl Pts',(-1.18625865667441,-1.,1.34687054001093));
#22258=CARTESIAN_POINT('Ctrl Pts',(-1.17501305789857,-1.,1.33437539347008));
#22259=CARTESIAN_POINT('Ctrl Pts',(-1.16589330093588,-1.,1.32428080721772));
#22260=CARTESIAN_POINT('Ctrl Pts',(-1.15950888730809,-1.,1.31722977216397));
#22261=CARTESIAN_POINT('Ctrl Pts',(-1.15624053661742,-1.,1.31362392696032));
#22262=CARTESIAN_POINT('',(-1.31362392696033,-1.,1.15624053661742));
#22263=CARTESIAN_POINT('Origin',(0.,-1.,0.));
#22264=CARTESIAN_POINT('',(-1.73811241238545,-1.,1.34869019493419));
#22265=CARTESIAN_POINT('Ctrl Pts',(-1.31362392696033,-1.,1.15624053661742));
#22266=CARTESIAN_POINT('Ctrl Pts',(-1.3172297721596,-1.,1.15950888730433));
#22267=CARTESIAN_POINT('Ctrl Pts',(-1.32428080720544,-1.,1.16589330092532));
#22268=CARTESIAN_POINT('Ctrl Pts',(-1.33437539344842,-1.,1.17501305787994));
#22269=CARTESIAN_POINT('Ctrl Pts',(-1.34687053998157,-1.,1.18625865664915));
#22270=CARTESIAN_POINT('Ctrl Pts',(-1.36088705040677,-1.,1.1987959077656));
#22271=CARTESIAN_POINT('Ctrl Pts',(-1.37331915604962,-1.,1.20982812923113));
#22272=CARTESIAN_POINT('Ctrl Pts',(-1.38420564525391,-1.,1.21938737278853));
#22273=CARTESIAN_POINT('Ctrl Pts',(-1.39361389567257,-1.,1.22752961898063));
#22274=CARTESIAN_POINT('Ctrl Pts',(-1.40164708205345,-1.,1.23434087289768));
#22275=CARTESIAN_POINT('Ctrl Pts',(-1.40845295531151,-1.,1.23994455029421));
#22276=CARTESIAN_POINT('Ctrl Pts',(-1.41422913175437,-1.,1.24450600513278));
#22277=CARTESIAN_POINT('Ctrl Pts',(-1.41923722596421,-1.,1.24824430986911));
#22278=CARTESIAN_POINT('Ctrl Pts',(-1.42378102115911,-1.,1.25141455570299));
#22279=CARTESIAN_POINT('Ctrl Pts',(-1.42815938799555,-1.,1.25426945222783));
#22280=CARTESIAN_POINT('Ctrl Pts',(-1.43262645609679,-1.,1.25702687965744));
#22281=CARTESIAN_POINT('Ctrl Pts',(-1.43734919180719,-1.,1.25983531011894));
#22282=CARTESIAN_POINT('Ctrl Pts',(-1.44236470511145,-1.,1.26273903323723));
#22283=CARTESIAN_POINT('Ctrl Pts',(-1.44761985001544,-1.,1.26570925118767));
#22284=CARTESIAN_POINT('Ctrl Pts',(-1.45301422764205,-1.,1.26867786804854));
#22285=CARTESIAN_POINT('Ctrl Pts',(-1.45843906294725,-1.,1.27156805265312));
#22286=CARTESIAN_POINT('Ctrl Pts',(-1.4638243133254,-1.,1.27433119897877));
#22287=CARTESIAN_POINT('Ctrl Pts',(-1.46916035917197,-1.,1.27696414831144));
#22288=CARTESIAN_POINT('Ctrl Pts',(-1.4744717526711,-1.,1.27948918248524));
#22289=CARTESIAN_POINT('Ctrl Pts',(-1.47980070347102,-1.,1.28194158939522));
#22290=CARTESIAN_POINT('Ctrl Pts',(-1.48518817118891,-1.,1.28435533880184));
#22291=CARTESIAN_POINT('Ctrl Pts',(-1.4906522831275,-1.,1.28674676116415));
#22292=CARTESIAN_POINT('Ctrl Pts',(-1.49618896881729,-1.,1.28911506584232));
#22293=CARTESIAN_POINT('Ctrl Pts',(-1.50178230149764,-1.,1.29145022885171));
#22294=CARTESIAN_POINT('Ctrl Pts',(-1.50741159078367,-1.,1.29373841372843));
#22295=CARTESIAN_POINT('Ctrl Pts',(-1.51305994241412,-1.,1.29596850710518));
#22296=CARTESIAN_POINT('Ctrl Pts',(-1.51872184912735,-1.,1.29813791800757));
#22297=CARTESIAN_POINT('Ctrl Pts',(-1.5243995786107,-1.,1.30024984366334));
#22298=CARTESIAN_POINT('Ctrl Pts',(-1.53009970283893,-1.,1.3023106439557));
#22299=CARTESIAN_POINT('Ctrl Pts',(-1.53582981268976,-1.,1.30432735639487));
#22300=CARTESIAN_POINT('Ctrl Pts',(-1.54159462645428,-1.,1.30630475189553));
#22301=CARTESIAN_POINT('Ctrl Pts',(-1.54739413957183,-1.,1.30824393907471));
#22302=CARTESIAN_POINT('Ctrl Pts',(-1.55322568759481,-1.,1.31014393684221));
#22303=CARTESIAN_POINT('Ctrl Pts',(-1.55908521254822,-1.,1.31200264341696));
#22304=CARTESIAN_POINT('Ctrl Pts',(-1.56496872402352,-1.,1.31381795281002));
#22305=CARTESIAN_POINT('Ctrl Pts',(-1.57087397835721,-1.,1.31558903860015));
#22306=CARTESIAN_POINT('Ctrl Pts',(-1.57680056505585,-1.,1.31731642317183));
#22307=CARTESIAN_POINT('Ctrl Pts',(-1.58274907898829,-1.,1.31900135021428));
#22308=CARTESIAN_POINT('Ctrl Pts',(-1.58872057258244,-1.,1.32064537110891));
#22309=CARTESIAN_POINT('Ctrl Pts',(-1.59471591079408,-1.,1.32224985747686));
#22310=CARTESIAN_POINT('Ctrl Pts',(-1.600735118587,-1.,1.32381550858266));
#22311=CARTESIAN_POINT('Ctrl Pts',(-1.6067775829097,-1.,1.32534250785794));
#22312=CARTESIAN_POINT('Ctrl Pts',(-1.61284234015762,-1.,1.32683074483365));
#22313=CARTESIAN_POINT('Ctrl Pts',(-1.61892832270723,-1.,1.32828000610448));
#22314=CARTESIAN_POINT('Ctrl Pts',(-1.62503464209777,-1.,1.32969019505665));
#22315=CARTESIAN_POINT('Ctrl Pts',(-1.63116079730887,-1.,1.33106149345618));
#22316=CARTESIAN_POINT('Ctrl Pts',(-1.6373065347505,-1.,1.33239425103694));
#22317=CARTESIAN_POINT('Ctrl Pts',(-1.64347174856007,-1.,1.33368890676554));
#22318=CARTESIAN_POINT('Ctrl Pts',(-1.64965637286843,-1.,1.33494590468003));
#22319=CARTESIAN_POINT('Ctrl Pts',(-1.65586025952651,-1.,1.33616559745217));
#22320=CARTESIAN_POINT('Ctrl Pts',(-1.66208312542073,-1.,1.33734820885331));
#22321=CARTESIAN_POINT('Ctrl Pts',(-1.66832460784078,-1.,1.33849388654458));
#22322=CARTESIAN_POINT('Ctrl Pts',(-1.67458429426126,-1.,1.33960273470372));
#22323=CARTESIAN_POINT('Ctrl Pts',(-1.68086176030308,-1.,1.3406748518516));
#22324=CARTESIAN_POINT('Ctrl Pts',(-1.68715660868602,-1.,1.34171037484673));
#22325=CARTESIAN_POINT('Ctrl Pts',(-1.6934684849664,-1.,1.34270948206139));
#22326=CARTESIAN_POINT('Ctrl Pts',(-1.69979707754221,-1.,1.34367237124322));
#22327=CARTESIAN_POINT('Ctrl Pts',(-1.70614212266676,-1.,1.34459924533783));
#22328=CARTESIAN_POINT('Ctrl Pts',(-1.71250340687011,-1.,1.34549029589563));
#22329=CARTESIAN_POINT('Ctrl Pts',(-1.7188807715095,-1.,1.34634568653586));
#22330=CARTESIAN_POINT('Ctrl Pts',(-1.72527410681298,-1.,1.34716554820013));
#22331=CARTESIAN_POINT('Ctrl Pts',(-1.73040149654497,-1.,1.3477930915247));
#22332=CARTESIAN_POINT('Ctrl Pts',(-1.73425417886255,-1.,1.34824783113158));
#22333=CARTESIAN_POINT('Ctrl Pts',(-1.73682580585819,-1.,1.34854391898145));
#22334=CARTESIAN_POINT('Ctrl Pts',(-1.73811241238545,-1.,1.34869019493419));
#22335=CARTESIAN_POINT('',(-1.81978687191668,-1.,1.23627494547115));
#22336=CARTESIAN_POINT('',(-1.73811241238545,-1.,1.34869019493419));
#22337=CARTESIAN_POINT('',(-1.5055822144029,-1.,0.892032620296855));
#22338=CARTESIAN_POINT('Ctrl Pts',(-1.81978687191668,-1.,1.23627494547115));
#22339=CARTESIAN_POINT('Ctrl Pts',(-1.81925017193531,-1.,1.23509651170384));
#22340=CARTESIAN_POINT('Ctrl Pts',(-1.81817389920914,-1.,1.23274224526804));
#22341=CARTESIAN_POINT('Ctrl Pts',(-1.81655087183054,-1.,1.22921864890975));
#22342=CARTESIAN_POINT('Ctrl Pts',(-1.81436959209778,-1.,1.22453613304507));
#22343=CARTESIAN_POINT('Ctrl Pts',(-1.81161420806172,-1.,1.2187090610323));
#22344=CARTESIAN_POINT('Ctrl Pts',(-1.80882996916931,-1.,1.2129081570818));
#22345=CARTESIAN_POINT('Ctrl Pts',(-1.80601678480772,-1.,1.20713356605519));
#22346=CARTESIAN_POINT('Ctrl Pts',(-1.8031745483882,-1.,1.2013854893912));
#22347=CARTESIAN_POINT('Ctrl Pts',(-1.80030314370121,-1.,1.19566418930405));
#22348=CARTESIAN_POINT('Ctrl Pts',(-1.79740245923649,-1.,1.1899699793456));
#22349=CARTESIAN_POINT('Ctrl Pts',(-1.79447240321572,-1.,1.18430321697471));
#22350=CARTESIAN_POINT('Ctrl Pts',(-1.79151291552646,-1.,1.17866429440781));
#22351=CARTESIAN_POINT('Ctrl Pts',(-1.78852398877523,-1.,1.17305363177265));
#22352=CARTESIAN_POINT('Ctrl Pts',(-1.78550566040349,-1.,1.16747166312239));
#22353=CARTESIAN_POINT('Ctrl Pts',(-1.78245795880949,-1.,1.16191881298458));
#22354=CARTESIAN_POINT('Ctrl Pts',(-1.77938085564261,-1.,1.15639547194689));
#22355=CARTESIAN_POINT('Ctrl Pts',(-1.77627422557034,-1.,1.15090197841531));
#22356=CARTESIAN_POINT('Ctrl Pts',(-1.77313777896234,-1.,1.14543858226948));
#22357=CARTESIAN_POINT('Ctrl Pts',(-1.76997111386806,-1.,1.14000548337));
#22358=CARTESIAN_POINT('Ctrl Pts',(-1.76677384551883,-1.,1.13460291804635));
#22359=CARTESIAN_POINT('Ctrl Pts',(-1.76354571966171,-1.,1.12923123555076));
#22360=CARTESIAN_POINT('Ctrl Pts',(-1.76028671825084,-1.,1.12389096855078));
#22361=CARTESIAN_POINT('Ctrl Pts',(-1.75699720772089,-1.,1.11858293216752));
#22362=CARTESIAN_POINT('Ctrl Pts',(-1.75367772094617,-1.,1.11330807582542));
#22363=CARTESIAN_POINT('Ctrl Pts',(-1.75032866075914,-1.,1.10806728183003));
#22364=CARTESIAN_POINT('Ctrl Pts',(-1.74695004214924,-1.,1.10286118991144));
#22365=CARTESIAN_POINT('Ctrl Pts',(-1.74354119236212,-1.,1.09768999241229));
#22366=CARTESIAN_POINT('Ctrl Pts',(-1.74010053962252,-1.,1.09255329056496));
#22367=CARTESIAN_POINT('Ctrl Pts',(-1.73662628326093,-1.,1.08745056285429));
#22368=CARTESIAN_POINT('Ctrl Pts',(-1.73311705663407,-1.,1.08238162784749));
#22369=CARTESIAN_POINT('Ctrl Pts',(-1.72957248977424,-1.,1.0773470373727));
#22370=CARTESIAN_POINT('Ctrl Pts',(-1.72599406198489,-1.,1.07234866990252));
#22371=CARTESIAN_POINT('Ctrl Pts',(-1.72238500928456,-1.,1.06738966975463));
#22372=CARTESIAN_POINT('Ctrl Pts',(-1.71874858456908,-1.,1.0624732468065));
#22373=CARTESIAN_POINT('Ctrl Pts',(-1.71508654427022,-1.,1.05760163192481));
#22374=CARTESIAN_POINT('Ctrl Pts',(-1.71139783543986,-1.,1.05277517202854));
#22375=CARTESIAN_POINT('Ctrl Pts',(-1.70767646263641,-1.,1.0479908540499));
#22376=CARTESIAN_POINT('Ctrl Pts',(-1.70391338707969,-1.,1.04324363334546));
#22377=CARTESIAN_POINT('Ctrl Pts',(-1.70010052930951,-1.,1.03852922490782));
#22378=CARTESIAN_POINT('Ctrl Pts',(-1.69623414782769,-1.,1.03384646003587));
#22379=CARTESIAN_POINT('Ctrl Pts',(-1.69231840863471,-1.,1.02919977579155));
#22380=CARTESIAN_POINT('Ctrl Pts',(-1.68836910178475,-1.,1.02460180535272));
#22381=CARTESIAN_POINT('Ctrl Pts',(-1.68440578021739,-1.,1.02006795074222));
#22382=CARTESIAN_POINT('Ctrl Pts',(-1.6804428989482,-1.,1.01561026162787));
#22383=CARTESIAN_POINT('Ctrl Pts',(-1.67648246776457,-1.,1.01123236493507));
#22384=CARTESIAN_POINT('Ctrl Pts',(-1.67250335383248,-1.,1.00692206696387));
#22385=CARTESIAN_POINT('Ctrl Pts',(-1.66846059277231,-1.,1.00265091003682));
#22386=CARTESIAN_POINT('Ctrl Pts',(-1.66430758030304,-1.,0.998389654952317));
#22387=CARTESIAN_POINT('Ctrl Pts',(-1.66001553809916,-1.,0.994121836661116));
#22388=CARTESIAN_POINT('Ctrl Pts',(-1.65559044289746,-1.,0.98985562785445));
#22389=CARTESIAN_POINT('Ctrl Pts',(-1.6511001661277,-1.,0.985642622921626));
#22390=CARTESIAN_POINT('Ctrl Pts',(-1.64665139190834,-1.,0.981562530940574));
#22391=CARTESIAN_POINT('Ctrl Pts',(-1.64233990826831,-1.,0.977689794120297));
#22392=CARTESIAN_POINT('Ctrl Pts',(-1.63820952658157,-1.,0.974066058287501));
#22393=CARTESIAN_POINT('Ctrl Pts',(-1.63420665729609,-1.,0.970669715996356));
#22394=CARTESIAN_POINT('Ctrl Pts',(-1.63013849959083,-1.,0.967387853228041));
#22395=CARTESIAN_POINT('Ctrl Pts',(-1.6257193066974,-1.,0.964046107037821));
#22396=CARTESIAN_POINT('Ctrl Pts',(-1.62061638139929,-1.,0.960438326099958));
#22397=CARTESIAN_POINT('Ctrl Pts',(-1.61449324337233,-1.,0.956354422921573));
#22398=CARTESIAN_POINT('Ctrl Pts',(-1.60706069897794,-1.,0.951613284361248));
#22399=CARTESIAN_POINT('Ctrl Pts',(-1.59810042045408,-1.,0.946078063325796));
#22400=CARTESIAN_POINT('Ctrl Pts',(-1.58744937489796,-1.,0.939646377909319));
#22401=CARTESIAN_POINT('Ctrl Pts',(-1.57499388385561,-1.,0.932246680128849));
#22402=CARTESIAN_POINT('Ctrl Pts',(-1.56065988582509,-1.,0.923832188966322));
#22403=CARTESIAN_POINT('Ctrl Pts',(-1.54440491152808,-1.,0.91437591904658));
#22404=CARTESIAN_POINT('Ctrl Pts',(-1.52984849890434,-1.,0.905967409640499));
#22405=CARTESIAN_POINT('Ctrl Pts',(-1.51805569591479,-1.,0.89918504749193));
#22406=CARTESIAN_POINT('Ctrl Pts',(-1.50980486807181,-1.,0.894452006967538));
#22407=CARTESIAN_POINT('Ctrl Pts',(-1.5055822144029,-1.,0.892032620296855));
#22408=CARTESIAN_POINT('',(-1.60662857109684,-1.,0.693717979106305));
#22409=CARTESIAN_POINT('Origin',(0.,-1.,0.));
#22410=CARTESIAN_POINT('',(-2.0698113262342,-1.,0.7455743247944));
#22411=CARTESIAN_POINT('Ctrl Pts',(-1.60662857109684,-1.,0.693717979106305));
#22412=CARTESIAN_POINT('Ctrl Pts',(-1.61106790957619,-1.,0.69571209787897));
#22413=CARTESIAN_POINT('Ctrl Pts',(-1.61974673471117,-1.,0.699605146398837));
#22414=CARTESIAN_POINT('Ctrl Pts',(-1.6321654166204,-1.,0.705159151977294));
#22415=CARTESIAN_POINT('Ctrl Pts',(-1.64752408828442,-1.,0.711993139340447));
#22416=CARTESIAN_POINT('Ctrl Pts',(-1.66472880551777,-1.,0.71958543378795));
#22417=CARTESIAN_POINT('Ctrl Pts',(-1.67996158451922,-1.,0.726235967982445));
#22418=CARTESIAN_POINT('Ctrl Pts',(-1.69326921972915,-1.,0.731963238685357));
#22419=CARTESIAN_POINT('Ctrl Pts',(-1.70473309004249,-1.,0.736799665716932));
#22420=CARTESIAN_POINT('Ctrl Pts',(-1.71447789751001,-1.,0.74079516202821));
#22421=CARTESIAN_POINT('Ctrl Pts',(-1.72268229916769,-1.,0.744021445433093));
#22422=CARTESIAN_POINT('Ctrl Pts',(-1.72958533647714,-1.,0.746574710097752));
#22423=CARTESIAN_POINT('Ctrl Pts',(-1.7355035168033,-1.,0.74858246295687));
#22424=CARTESIAN_POINT('Ctrl Pts',(-1.74080458267114,-1.,0.750193435981249));
#22425=CARTESIAN_POINT('Ctrl Pts',(-1.74585086852502,-1.,0.751555614164482));
#22426=CARTESIAN_POINT('Ctrl Pts',(-1.75095139468794,-1.,0.752797683531314));
#22427=CARTESIAN_POINT('Ctrl Pts',(-1.75631083600019,-1.,0.754009254027829));
#22428=CARTESIAN_POINT('Ctrl Pts',(-1.76197817240128,-1.,0.755220979974461));
#22429=CARTESIAN_POINT('Ctrl Pts',(-1.76789396002998,-1.,0.75642189602781));
#22430=CARTESIAN_POINT('Ctrl Pts',(-1.77394167108292,-1.,0.757578264077029));
#22431=CARTESIAN_POINT('Ctrl Pts',(-1.77999411220945,-1.,0.758650626677518));
#22432=CARTESIAN_POINT('Ctrl Pts',(-1.78596964884604,-1.,0.759614401110189));
#22433=CARTESIAN_POINT('Ctrl Pts',(-1.7918581561088,-1.,0.760469555880749));
#22434=CARTESIAN_POINT('Ctrl Pts',(-1.79768986997783,-1.,0.761229695230558));
#22435=CARTESIAN_POINT('Ctrl Pts',(-1.80351583877342,-1.,0.761915336443547));
#22436=CARTESIAN_POINT('Ctrl Pts',(-1.80938551463965,-1.,0.762546129463938));
#22437=CARTESIAN_POINT('Ctrl Pts',(-1.8153211840553,-1.,0.763132003836634));
#22438=CARTESIAN_POINT('Ctrl Pts',(-1.82131873145266,-1.,0.763673465462726));
#22439=CARTESIAN_POINT('Ctrl Pts',(-1.82735991200065,-1.,0.764165902605995));
#22440=CARTESIAN_POINT('Ctrl Pts',(-1.83342077227142,-1.,0.764602549687853));
#22441=CARTESIAN_POINT('Ctrl Pts',(-1.83948181064835,-1.,0.764978057881737));
#22442=CARTESIAN_POINT('Ctrl Pts',(-1.84553698875924,-1.,0.765291664862029));
#22443=CARTESIAN_POINT('Ctrl Pts',(-1.85158945130063,-1.,0.765545710619062));
#22444=CARTESIAN_POINT('Ctrl Pts',(-1.85764741390394,-1.,0.765744212909318));
#22445=CARTESIAN_POINT('Ctrl Pts',(-1.86372027063312,-1.,0.765891519092547));
#22446=CARTESIAN_POINT('Ctrl Pts',(-1.86981398314341,-1.,0.765990708546091));
#22447=CARTESIAN_POINT('Ctrl Pts',(-1.87592888967883,-1.,0.766042837036744));
#22448=CARTESIAN_POINT('Ctrl Pts',(-1.88206215302561,-1.,0.766047794851864));
#22449=CARTESIAN_POINT('Ctrl Pts',(-1.88820926433409,-1.,0.766004837062091));
#22450=CARTESIAN_POINT('Ctrl Pts',(-1.89436577771388,-1.,0.765913193856978));
#22451=CARTESIAN_POINT('Ctrl Pts',(-1.90052930393596,-1.,0.765772772593386));
#22452=CARTESIAN_POINT('Ctrl Pts',(-1.90669961402356,-1.,0.765584196937919));
#22453=CARTESIAN_POINT('Ctrl Pts',(-1.91287765805169,-1.,0.765348465884722));
#22454=CARTESIAN_POINT('Ctrl Pts',(-1.91906491634196,-1.,0.765066729667088));
#22455=CARTESIAN_POINT('Ctrl Pts',(-1.92526263537048,-1.,0.764740025488211));
#22456=CARTESIAN_POINT('Ctrl Pts',(-1.93147105496382,-1.,0.76436901067394));
#22457=CARTESIAN_POINT('Ctrl Pts',(-1.93768964875886,-1.,0.763954049121458));
#22458=CARTESIAN_POINT('Ctrl Pts',(-1.9439174661764,-1.,0.763495333538629));
#22459=CARTESIAN_POINT('Ctrl Pts',(-1.95015342590024,-1.,0.762992990878769));
#22460=CARTESIAN_POINT('Ctrl Pts',(-1.95639665309869,-1.,0.762447203806179));
#22461=CARTESIAN_POINT('Ctrl Pts',(-1.96264672744186,-1.,0.761858300014423));
#22462=CARTESIAN_POINT('Ctrl Pts',(-1.96890351582499,-1.,0.76122669048382));
#22463=CARTESIAN_POINT('Ctrl Pts',(-1.97516705321494,-1.,0.760552825409757));
#22464=CARTESIAN_POINT('Ctrl Pts',(-1.98143741418172,-1.,0.75983714745219));
#22465=CARTESIAN_POINT('Ctrl Pts',(-1.98771456680874,-1.,0.759080037802488));
#22466=CARTESIAN_POINT('Ctrl Pts',(-1.99399831098817,-1.,0.758281796766761));
#22467=CARTESIAN_POINT('Ctrl Pts',(-2.00028834739178,-1.,0.757442676862724));
#22468=CARTESIAN_POINT('Ctrl Pts',(-2.0065843158773,-1.,0.75656290464667));
#22469=CARTESIAN_POINT('Ctrl Pts',(-2.01288584328084,-1.,0.755642704957865));
#22470=CARTESIAN_POINT('Ctrl Pts',(-2.01919259405809,-1.,0.754682330722816));
#22471=CARTESIAN_POINT('Ctrl Pts',(-2.02550428623313,-1.,0.753682061112768));
#22472=CARTESIAN_POINT('Ctrl Pts',(-2.03182068456221,-1.,0.752642180487211));
#22473=CARTESIAN_POINT('Ctrl Pts',(-2.03814160092099,-1.,0.751562963361115));
#22474=CARTESIAN_POINT('Ctrl Pts',(-2.04446689147979,-1.,0.750444657875576));
#22475=CARTESIAN_POINT('Ctrl Pts',(-2.05079645592154,-1.,0.749287468665046));
#22476=CARTESIAN_POINT('Ctrl Pts',(-2.05713023031006,-1.,0.748091554183802));
#22477=CARTESIAN_POINT('Ctrl Pts',(-2.06220058927826,-1.,0.747103932787919));
#22478=CARTESIAN_POINT('Ctrl Pts',(-2.06600523016815,-1.,0.7463458715442));
#22479=CARTESIAN_POINT('Ctrl Pts',(-2.06854248895728,-1.,0.745832791378367));
#22480=CARTESIAN_POINT('Ctrl Pts',(-2.0698113262342,-1.,0.7455743247944));
#22481=CARTESIAN_POINT('',(-2.11275013067528,-1.,0.61342227326009));
#22482=CARTESIAN_POINT('',(-2.0698113262342,-1.,0.7455743247944));
#22483=CARTESIAN_POINT('',(-1.7075470150345,-1.,0.383122945602004));
#22484=CARTESIAN_POINT('Ctrl Pts',(-2.11275013067528,-1.,0.61342227326009));
#22485=CARTESIAN_POINT('Ctrl Pts',(-2.11187554259986,-1.,0.6124673655618));
#22486=CARTESIAN_POINT('Ctrl Pts',(-2.11012443807238,-1.,0.610560911689899));
#22487=CARTESIAN_POINT('Ctrl Pts',(-2.1074919961518,-1.,0.607711315454876));
#22488=CARTESIAN_POINT('Ctrl Pts',(-2.10397049886949,-1.,0.60393203073603));
#22489=CARTESIAN_POINT('Ctrl Pts',(-2.0995493086477,-1.,0.599241616420533));
#22490=CARTESIAN_POINT('Ctrl Pts',(-2.0951087622027,-1.,0.594585006052162));
#22491=CARTESIAN_POINT('Ctrl Pts',(-2.09064881812129,-1.,0.589962365403406));
#22492=CARTESIAN_POINT('Ctrl Pts',(-2.08616943727951,-1.,0.585373918991617));
#22493=CARTESIAN_POINT('Ctrl Pts',(-2.08167059018418,-1.,0.580819952108063));
#22494=CARTESIAN_POINT('Ctrl Pts',(-2.07715226767559,-1.,0.576300797416844));
#22495=CARTESIAN_POINT('Ctrl Pts',(-2.07261449292824,-1.,0.571816823242603));
#22496=CARTESIAN_POINT('Ctrl Pts',(-2.06805732997334,-1.,0.567368421181087));
#22497=CARTESIAN_POINT('Ctrl Pts',(-2.06348090160589,-1.,0.562955993082261));
#22498=CARTESIAN_POINT('Ctrl Pts',(-2.05888537756462,-1.,0.558579940185151));
#22499=CARTESIAN_POINT('Ctrl Pts',(-2.05427091604413,-1.,0.554240657463906));
#22500=CARTESIAN_POINT('Ctrl Pts',(-2.04963761077958,-1.,0.549938525150295));
#22501=CARTESIAN_POINT('Ctrl Pts',(-2.04498544714588,-1.,0.54567390381743));
#22502=CARTESIAN_POINT('Ctrl Pts',(-2.04031422690527,-1.,0.541447120615659));
#22503=CARTESIAN_POINT('Ctrl Pts',(-2.03562362954037,-1.,0.537258489833262));
#22504=CARTESIAN_POINT('Ctrl Pts',(-2.03091336214426,-1.,0.533108355132976));
#22505=CARTESIAN_POINT('Ctrl Pts',(-2.0261832908329,-1.,0.528997127241914));
#22506=CARTESIAN_POINT('Ctrl Pts',(-2.02143356304698,-1.,0.524925318333476));
#22507=CARTESIAN_POINT('Ctrl Pts',(-2.01666477917286,-1.,0.52089359039937));
#22508=CARTESIAN_POINT('Ctrl Pts',(-2.01187773939242,-1.,0.516902681728687));
#22509=CARTESIAN_POINT('Ctrl Pts',(-2.00707309946949,-1.,0.512953306961792));
#22510=CARTESIAN_POINT('Ctrl Pts',(-2.00225107134734,-1.,0.509046069886157));
#22511=CARTESIAN_POINT('Ctrl Pts',(-1.99741107463572,-1.,0.505181361323026));
#22512=CARTESIAN_POINT('Ctrl Pts',(-1.99255149126155,-1.,0.501359287727146));
#22513=CARTESIAN_POINT('Ctrl Pts',(-1.98767044752932,-1.,0.497579909545574));
#22514=CARTESIAN_POINT('Ctrl Pts',(-1.98276658761821,-1.,0.493843476541494));
#22515=CARTESIAN_POINT('Ctrl Pts',(-1.97783973019229,-1.,0.490150627860952));
#22516=CARTESIAN_POINT('Ctrl Pts',(-1.97289186263272,-1.,0.486502692907659));
#22517=CARTESIAN_POINT('Ctrl Pts',(-1.96792703422362,-1.,0.48290166212069));
#22518=CARTESIAN_POINT('Ctrl Pts',(-1.96294933055943,-1.,0.479349583074855));
#22519=CARTESIAN_POINT('Ctrl Pts',(-1.95796111148177,-1.,0.475848034683176));
#22520=CARTESIAN_POINT('Ctrl Pts',(-1.95296148278133,-1.,0.472397672264072));
#22521=CARTESIAN_POINT('Ctrl Pts',(-1.94794381136514,-1.,0.468997482913135));
#22522=CARTESIAN_POINT('Ctrl Pts',(-1.9428979419619,-1.,0.46564546202603));
#22523=CARTESIAN_POINT('Ctrl Pts',(-1.93781486640821,-1.,0.462340031009056));
#22524=CARTESIAN_POINT('Ctrl Pts',(-1.93269066517934,-1.,0.459081234547926));
#22525=CARTESIAN_POINT('Ctrl Pts',(-1.92753067150476,-1.,0.455872005174371));
#22526=CARTESIAN_POINT('Ctrl Pts',(-1.92235380648502,-1.,0.452719478359432));
#22527=CARTESIAN_POINT('Ctrl Pts',(-1.91718342555755,-1.,0.449632260106662));
#22528=CARTESIAN_POINT('Ctrl Pts',(-1.9120369998112,-1.,0.446617343485711));
#22529=CARTESIAN_POINT('Ctrl Pts',(-1.90691756144898,-1.,0.44367755684915));
#22530=CARTESIAN_POINT('Ctrl Pts',(-1.90180124389086,-1.,0.440807833704038));
#22531=CARTESIAN_POINT('Ctrl Pts',(-1.89663648956466,-1.,0.437995003948244));
#22532=CARTESIAN_POINT('Ctrl Pts',(-1.89136993975504,-1.,0.435225660963383));
#22533=CARTESIAN_POINT('Ctrl Pts',(-1.88596913666793,-1.,0.432493038548748));
#22534=CARTESIAN_POINT('Ctrl Pts',(-1.88044229001832,-1.,0.429803062482344));
#22535=CARTESIAN_POINT('Ctrl Pts',(-1.87486989291484,-1.,0.427183828519102));
#22536=CARTESIAN_POINT('Ctrl Pts',(-1.86937803944323,-1.,0.424678177291359));
#22537=CARTESIAN_POINT('Ctrl Pts',(-1.86408083334028,-1.,0.422327307418275));
#22538=CARTESIAN_POINT('Ctrl Pts',(-1.85903281096686,-1.,0.420157287975619));
#22539=CARTESIAN_POINT('Ctrl Pts',(-1.85417632856234,-1.,0.418164129143534));
#22540=CARTESIAN_POINT('Ctrl Pts',(-1.84929312929882,-1.,0.416300022038864));
#22541=CARTESIAN_POINT('Ctrl Pts',(-1.8440575707371,-1.,0.41448743825434));
#22542=CARTESIAN_POINT('Ctrl Pts',(-1.83808953475839,-1.,0.412633125322161));
#22543=CARTESIAN_POINT('Ctrl Pts',(-1.83100408895216,-1.,0.410641256301675));
#22544=CARTESIAN_POINT('Ctrl Pts',(-1.8224702267854,-1.,0.408428948108533));
#22545=CARTESIAN_POINT('Ctrl Pts',(-1.81223801813988,-1.,0.405933518411838));
#22546=CARTESIAN_POINT('Ctrl Pts',(-1.80012077176221,-1.,0.403107976170441));
#22547=CARTESIAN_POINT('Ctrl Pts',(-1.78598826347533,-1.,0.39991940378308));
#22548=CARTESIAN_POINT('Ctrl Pts',(-1.7697556004756,-1.,0.39634619612042));
#22549=CARTESIAN_POINT('Ctrl Pts',(-1.75137405313962,-1.,0.392375812294307));
#22550=CARTESIAN_POINT('Ctrl Pts',(-1.7349317097561,-1.,0.388877023509191));
#22551=CARTESIAN_POINT('Ctrl Pts',(-1.72162022246158,-1.,0.38607079032701));
#22552=CARTESIAN_POINT('Ctrl Pts',(-1.71231062891958,-1.,0.384119047315542));
#22553=CARTESIAN_POINT('Ctrl Pts',(-1.7075470150345,-1.,0.383122945602004));
#22554=CARTESIAN_POINT('',(-1.74236521665491,-1.,0.163289472382896));
#22555=CARTESIAN_POINT('Origin',(0.,-1.,0.));
#22556=CARTESIAN_POINT('',(-2.19890268624765,-1.,0.069476445021958));
#22557=CARTESIAN_POINT('Ctrl Pts',(-1.74236521665491,-1.,0.163289472382896));
#22558=CARTESIAN_POINT('Ctrl Pts',(-1.7472034950333,-1.,0.163814161002002));
#22559=CARTESIAN_POINT('Ctrl Pts',(-1.75666056638427,-1.,0.164834765707158));
#22560=CARTESIAN_POINT('Ctrl Pts',(-1.77018771684844,-1.,0.1662793551464));
#22561=CARTESIAN_POINT('Ctrl Pts',(-1.7869064998507,-1.,0.168032772805197));
#22562=CARTESIAN_POINT('Ctrl Pts',(-1.80561530629706,-1.,0.169936923904608));
#22563=CARTESIAN_POINT('Ctrl Pts',(-1.82215766811545,-1.,0.171554770204119));
#22564=CARTESIAN_POINT('Ctrl Pts',(-1.83658380527692,-1.,0.1728894428919));
#22565=CARTESIAN_POINT('Ctrl Pts',(-1.8489811319852,-1.,0.173946627587731));
#22566=CARTESIAN_POINT('Ctrl Pts',(-1.85948367088837,-1.,0.17473525927603));
#22567=CARTESIAN_POINT('Ctrl Pts',(-1.86828349694799,-1.,0.175268337590758));
#22568=CARTESIAN_POINT('Ctrl Pts',(-1.87563767773588,-1.,0.175563480746485));
#22569=CARTESIAN_POINT('Ctrl Pts',(-1.88188663145367,-1.,0.175644148889698));
#22570=CARTESIAN_POINT('Ctrl Pts',(-1.88742606273259,-1.,0.175538155840648));
#22571=CARTESIAN_POINT('Ctrl Pts',(-1.892646301985,-1.,0.175274276190844));
#22572=CARTESIAN_POINT('Ctrl Pts',(-1.89788101117132,-1.,0.174879405091263));
#22573=CARTESIAN_POINT('Ctrl Pts',(-1.90335253862834,-1.,0.174375518661085));
#22574=CARTESIAN_POINT('Ctrl Pts',(-1.90911693975267,-1.,0.173776635257817));
#22575=CARTESIAN_POINT('Ctrl Pts',(-1.91511429159527,-1.,0.173090695383496));
#22576=CARTESIAN_POINT('Ctrl Pts',(-1.9212233439798,-1.,0.172321621259514));
#22577=CARTESIAN_POINT('Ctrl Pts',(-1.92731093582036,-1.,0.171471191532988));
#22578=CARTESIAN_POINT('Ctrl Pts',(-1.93329183155539,-1.,0.170541253116201));
#22579=CARTESIAN_POINT('Ctrl Pts',(-1.93915639211581,-1.,0.169534904817491));
#22580=CARTESIAN_POINT('Ctrl Pts',(-1.94493757756931,-1.,0.168455741607556));
#22581=CARTESIAN_POINT('Ctrl Pts',(-1.95069027794294,-1.,0.167307501784475));
#22582=CARTESIAN_POINT('Ctrl Pts',(-1.9564675971873,-1.,0.166093592002812));
#22583=CARTESIAN_POINT('Ctrl Pts',(-1.96229379940136,-1.,0.164816568920269));
#22584=CARTESIAN_POINT('Ctrl Pts',(-1.96816512677967,-1.,0.163478185457734));
#22585=CARTESIAN_POINT('Ctrl Pts',(-1.97406280235188,-1.,0.162079693556288));
#22586=CARTESIAN_POINT('Ctrl Pts',(-1.97996195437559,-1.,0.160622060784611));
#22587=CARTESIAN_POINT('Ctrl Pts',(-1.98584238283292,-1.,0.159106226437299));
#22588=CARTESIAN_POINT('Ctrl Pts',(-1.99169810931908,-1.,0.157533331459227));
#22589=CARTESIAN_POINT('Ctrl Pts',(-1.99753284771497,-1.,0.155904629548783));
#22590=CARTESIAN_POINT('Ctrl Pts',(-2.00335565310543,-1.,0.154221403049722));
#22591=CARTESIAN_POINT('Ctrl Pts',(-2.00917680318424,-1.,0.15248488362145));
#22592=CARTESIAN_POINT('Ctrl Pts',(-2.01500291940238,-1.,0.150696157673078));
#22593=CARTESIAN_POINT('Ctrl Pts',(-2.02083464969894,-1.,0.148856124775337));
#22594=CARTESIAN_POINT('Ctrl Pts',(-2.02666926182017,-1.,0.146965557332583));
#22595=CARTESIAN_POINT('Ctrl Pts',(-2.03250223739942,-1.,0.145025140186057));
#22596=CARTESIAN_POINT('Ctrl Pts',(-2.03832911025912,-1.,0.143035515058209));
#22597=CARTESIAN_POINT('Ctrl Pts',(-2.04414757947916,-1.,0.140997332152546));
#22598=CARTESIAN_POINT('Ctrl Pts',(-2.04995762001328,-1.,0.138911255368966));
#22599=CARTESIAN_POINT('Ctrl Pts',(-2.05576044414264,-1.,0.136777941218043));
#22600=CARTESIAN_POINT('Ctrl Pts',(-2.06155781517842,-1.,0.134598026192106));
#22601=CARTESIAN_POINT('Ctrl Pts',(-2.06735123910326,-1.,0.13237211154771));
#22602=CARTESIAN_POINT('Ctrl Pts',(-2.07314114713063,-1.,0.130100748328403));
#22603=CARTESIAN_POINT('Ctrl Pts',(-2.07892715110987,-1.,0.12778444527612));
#22604=CARTESIAN_POINT('Ctrl Pts',(-2.08470840653643,-1.,0.125423679412061));
#22605=CARTESIAN_POINT('Ctrl Pts',(-2.09048392424825,-1.,0.123018905621083));
#22606=CARTESIAN_POINT('Ctrl Pts',(-2.0962529286773,-1.,0.120570567965122));
#22607=CARTESIAN_POINT('Ctrl Pts',(-2.102015121329,-1.,0.118079107988355));
#22608=CARTESIAN_POINT('Ctrl Pts',(-2.10777050261309,-1.,0.115544957687926));
#22609=CARTESIAN_POINT('Ctrl Pts',(-2.11351924490306,-1.,0.112968534419737));
#22610=CARTESIAN_POINT('Ctrl Pts',(-2.11926155590865,-1.,0.110350236135025));
#22611=CARTESIAN_POINT('Ctrl Pts',(-2.12499752307,-1.,0.10769043523109));
#22612=CARTESIAN_POINT('Ctrl Pts',(-2.13072704887293,-1.,0.104989479152739));
#22613=CARTESIAN_POINT('Ctrl Pts',(-2.13644992667165,-1.,0.1022477005561));
#22614=CARTESIAN_POINT('Ctrl Pts',(-2.14216588396025,-1.,0.0994654261990914));
#22615=CARTESIAN_POINT('Ctrl Pts',(-2.14787463531795,-1.,0.0966429852305457));
#22616=CARTESIAN_POINT('Ctrl Pts',(-2.1535759397817,-1.,0.0937807218867642));
#22617=CARTESIAN_POINT('Ctrl Pts',(-2.15926961544516,-1.,0.0908789888107264));
#22618=CARTESIAN_POINT('Ctrl Pts',(-2.16495552645014,-1.,0.0879381291386921));
#22619=CARTESIAN_POINT('Ctrl Pts',(-2.17063357870952,-1.,0.0849584620835371));
#22620=CARTESIAN_POINT('Ctrl Pts',(-2.176303712113,-1.,0.0819402680872764));
#22621=CARTESIAN_POINT('Ctrl Pts',(-2.18196589448887,-1.,0.0788837727685241));
#22622=CARTESIAN_POINT('Ctrl Pts',(-2.1876201139953,-1.,0.0757891465836146));
#22623=CARTESIAN_POINT('Ctrl Pts',(-2.19213712013662,-1.,0.0732830357306724));
#22624=CARTESIAN_POINT('Ctrl Pts',(-2.19552129484002,-1.,0.0713863779526153));
#22625=CARTESIAN_POINT('Ctrl Pts',(-2.19777582085423,-1.,0.0701143536325489));
#22626=CARTESIAN_POINT('Ctrl Pts',(-2.19890268624765,-1.,0.069476445021958));
#22627=CARTESIAN_POINT('',(-2.19890268624765,-1.,-0.0694764450219585));
#22628=CARTESIAN_POINT('',(-2.19890268624765,-1.,0.069476445021958));
#22629=CARTESIAN_POINT('',(-1.74236521665491,-1.,-0.163289472382896));
#22630=CARTESIAN_POINT('Ctrl Pts',(-2.19890268624765,-1.,-0.0694764450219585));
#22631=CARTESIAN_POINT('Ctrl Pts',(-2.19777582085261,-1.,-0.0701143536324927));
#22632=CARTESIAN_POINT('Ctrl Pts',(-2.19552129483562,-1.,-0.0713863779524629));
#22633=CARTESIAN_POINT('Ctrl Pts',(-2.19213712012956,-1.,-0.0732830357304277));
#22634=CARTESIAN_POINT('Ctrl Pts',(-2.1876201139874,-1.,-0.0757891465833413));
#22635=CARTESIAN_POINT('Ctrl Pts',(-2.18196589448304,-1.,-0.0788837727683229));
#22636=CARTESIAN_POINT('Ctrl Pts',(-2.1763037121106,-1.,-0.0819402680871941));
#22637=CARTESIAN_POINT('Ctrl Pts',(-2.17063357871031,-1.,-0.0849584620835644));
#22638=CARTESIAN_POINT('Ctrl Pts',(-2.16495552645275,-1.,-0.0879381291387824));
#22639=CARTESIAN_POINT('Ctrl Pts',(-2.15926961544808,-1.,-0.0908789888108267));
#22640=CARTESIAN_POINT('Ctrl Pts',(-2.15357593978377,-1.,-0.0937807218868346));
#22641=CARTESIAN_POINT('Ctrl Pts',(-2.14787463531864,-1.,-0.096642985230569));
#22642=CARTESIAN_POINT('Ctrl Pts',(-2.14216588395974,-1.,-0.0994654261990744));
#22643=CARTESIAN_POINT('Ctrl Pts',(-2.13644992667052,-1.,-0.102247700556064));
#22644=CARTESIAN_POINT('Ctrl Pts',(-2.1307270488718,-1.,-0.104989479152703));
#22645=CARTESIAN_POINT('Ctrl Pts',(-2.12499752306927,-1.,-0.107690435231068));
#22646=CARTESIAN_POINT('Ctrl Pts',(-2.11926155590849,-1.,-0.11035023613502));
#22647=CARTESIAN_POINT('Ctrl Pts',(-2.11351924490335,-1.,-0.112968534419746));
#22648=CARTESIAN_POINT('Ctrl Pts',(-2.10777050261359,-1.,-0.11554495768794));
#22649=CARTESIAN_POINT('Ctrl Pts',(-2.10201512132945,-1.,-0.118079107988368));
#22650=CARTESIAN_POINT('Ctrl Pts',(-2.09625292867756,-1.,-0.120570567965129));
#22651=CARTESIAN_POINT('Ctrl Pts',(-2.09048392424826,-1.,-0.123018905621083));
#22652=CARTESIAN_POINT('Ctrl Pts',(-2.08470840653628,-1.,-0.125423679412058));
#22653=CARTESIAN_POINT('Ctrl Pts',(-2.07892715110967,-1.,-0.127784445276116));
#22654=CARTESIAN_POINT('Ctrl Pts',(-2.07314114713047,-1.,-0.130100748328401));
#22655=CARTESIAN_POINT('Ctrl Pts',(-2.06735123910319,-1.,-0.13237211154771));
#22656=CARTESIAN_POINT('Ctrl Pts',(-2.06155781517844,-1.,-0.134598026192107));
#22657=CARTESIAN_POINT('Ctrl Pts',(-2.0557604441427,-1.,-0.136777941218044));
#22658=CARTESIAN_POINT('Ctrl Pts',(-2.04995762001333,-1.,-0.138911255368966));
#22659=CARTESIAN_POINT('Ctrl Pts',(-2.04414757947919,-1.,-0.140997332152545));
#22660=CARTESIAN_POINT('Ctrl Pts',(-2.03832911025913,-1.,-0.143035515058208));
#22661=CARTESIAN_POINT('Ctrl Pts',(-2.03250223739941,-1.,-0.145025140186058));
#22662=CARTESIAN_POINT('Ctrl Pts',(-2.02666926182017,-1.,-0.146965557332586));
#22663=CARTESIAN_POINT('Ctrl Pts',(-2.02083464969897,-1.,-0.148856124775343));
#22664=CARTESIAN_POINT('Ctrl Pts',(-2.01500291940243,-1.,-0.150696157673084));
#22665=CARTESIAN_POINT('Ctrl Pts',(-2.00917680318426,-1.,-0.152484883621452));
#22666=CARTESIAN_POINT('Ctrl Pts',(-2.00335565310539,-1.,-0.154221403049719));
#22667=CARTESIAN_POINT('Ctrl Pts',(-1.99753284771487,-1.,-0.155904629548775));
#22668=CARTESIAN_POINT('Ctrl Pts',(-1.99169810931893,-1.,-0.157533331459215));
#22669=CARTESIAN_POINT('Ctrl Pts',(-1.98584238283279,-1.,-0.159106226437289));
#22670=CARTESIAN_POINT('Ctrl Pts',(-1.97996195437557,-1.,-0.16062206078461));
#22671=CARTESIAN_POINT('Ctrl Pts',(-1.97406280235204,-1.,-0.162079693556302));
#22672=CARTESIAN_POINT('Ctrl Pts',(-1.96816512678,-1.,-0.16347818545776));
#22673=CARTESIAN_POINT('Ctrl Pts',(-1.96229379940174,-1.,-0.1648165689203));
#22674=CARTESIAN_POINT('Ctrl Pts',(-1.95646759718755,-1.,-0.166093592002833));
#22675=CARTESIAN_POINT('Ctrl Pts',(-1.95069027794286,-1.,-0.167307501784469));
#22676=CARTESIAN_POINT('Ctrl Pts',(-1.94493757756879,-1.,-0.168455741607516));
#22677=CARTESIAN_POINT('Ctrl Pts',(-1.93915639211497,-1.,-0.169534904817425));
#22678=CARTESIAN_POINT('Ctrl Pts',(-1.93329183155455,-1.,-0.170541253116136));
#22679=CARTESIAN_POINT('Ctrl Pts',(-1.92731093582,-1.,-0.17147119153296));
#22680=CARTESIAN_POINT('Ctrl Pts',(-1.92122334398034,-1.,-0.172321621259557));
#22681=CARTESIAN_POINT('Ctrl Pts',(-1.91511429159681,-1.,-0.173090695383619));
#22682=CARTESIAN_POINT('Ctrl Pts',(-1.90911693975475,-1.,-0.173776635257984));
#22683=CARTESIAN_POINT('Ctrl Pts',(-1.90335253863003,-1.,-0.174375518661222));
#22684=CARTESIAN_POINT('Ctrl Pts',(-1.89788101117148,-1.,-0.174879405091277));
#22685=CARTESIAN_POINT('Ctrl Pts',(-1.89264630198279,-1.,-0.175274276190664));
#22686=CARTESIAN_POINT('Ctrl Pts',(-1.88742606272818,-1.,-0.175538155840286));
#22687=CARTESIAN_POINT('Ctrl Pts',(-1.88188663144846,-1.,-0.175644148889271));
#22688=CARTESIAN_POINT('Ctrl Pts',(-1.87563767773249,-1.,-0.175563480746205));
#22689=CARTESIAN_POINT('Ctrl Pts',(-1.86828349694972,-1.,-0.175268337590901));
#22690=CARTESIAN_POINT('Ctrl Pts',(-1.85948367089838,-1.,-0.174735259276856));
#22691=CARTESIAN_POINT('Ctrl Pts',(-1.84898113200543,-1.,-0.173946627589401));
#22692=CARTESIAN_POINT('Ctrl Pts',(-1.83658380530747,-1.,-0.17288944289442));
#22693=CARTESIAN_POINT('Ctrl Pts',(-1.82215766815414,-1.,-0.171554770207306));
#22694=CARTESIAN_POINT('Ctrl Pts',(-1.80561530633924,-1.,-0.169936923908078));
#22695=CARTESIAN_POINT('Ctrl Pts',(-1.78690649988931,-1.,-0.16803277280837));
#22696=CARTESIAN_POINT('Ctrl Pts',(-1.77018771687692,-1.,-0.166279355148738));
#22697=CARTESIAN_POINT('Ctrl Pts',(-1.75666056640041,-1.,-0.164834765708484));
#22698=CARTESIAN_POINT('Ctrl Pts',(-1.74720349503904,-1.,-0.163814161002474));
#22699=CARTESIAN_POINT('Ctrl Pts',(-1.74236521665491,-1.,-0.163289472382896));
#22700=CARTESIAN_POINT('',(-1.7075470150345,-1.,-0.383122945602004));
#22701=CARTESIAN_POINT('Origin',(0.,-1.,0.));
#22702=CARTESIAN_POINT('',(-2.11275013067528,-1.,-0.61342227326009));
#22703=CARTESIAN_POINT('Ctrl Pts',(-1.7075470150345,-1.,-0.383122945602004));
#22704=CARTESIAN_POINT('Ctrl Pts',(-1.71231062891398,-1.,-0.384119047314215));
#22705=CARTESIAN_POINT('Ctrl Pts',(-1.72162022244582,-1.,-0.386070790323281));
#22706=CARTESIAN_POINT('Ctrl Pts',(-1.73493170972829,-1.,-0.388877023502615));
#22707=CARTESIAN_POINT('Ctrl Pts',(-1.75137405310193,-1.,-0.392375812285395));
#22708=CARTESIAN_POINT('Ctrl Pts',(-1.76975560043442,-1.,-0.396346196110688));
#22709=CARTESIAN_POINT('Ctrl Pts',(-1.78598826343754,-1.,-0.399919403774155));
#22710=CARTESIAN_POINT('Ctrl Pts',(-1.80012077173238,-1.,-0.403107976163396));
#22711=CARTESIAN_POINT('Ctrl Pts',(-1.81223801812013,-1.,-0.405933518407175));
#22712=CARTESIAN_POINT('Ctrl Pts',(-1.82247022677562,-1.,-0.408428948106227));
#22713=CARTESIAN_POINT('Ctrl Pts',(-1.83100408895047,-1.,-0.410641256301276));
#22714=CARTESIAN_POINT('Ctrl Pts',(-1.8380895347617,-1.,-0.412633125322945));
#22715=CARTESIAN_POINT('Ctrl Pts',(-1.84405757074218,-1.,-0.414487438255542));
#22716=CARTESIAN_POINT('Ctrl Pts',(-1.84929312930314,-1.,-0.416300022039885));
#22717=CARTESIAN_POINT('Ctrl Pts',(-1.8541763285645,-1.,-0.418164129144045));
#22718=CARTESIAN_POINT('Ctrl Pts',(-1.8590328109667,-1.,-0.420157287975583));
#22719=CARTESIAN_POINT('Ctrl Pts',(-1.86408083333863,-1.,-0.422327307417884));
#22720=CARTESIAN_POINT('Ctrl Pts',(-1.8693780394412,-1.,-0.424678177290876));
#22721=CARTESIAN_POINT('Ctrl Pts',(-1.87486989291333,-1.,-0.427183828518743));
#22722=CARTESIAN_POINT('Ctrl Pts',(-1.88044229001778,-1.,-0.429803062482217));
#22723=CARTESIAN_POINT('Ctrl Pts',(-1.88596913666828,-1.,-0.432493038548833));
#22724=CARTESIAN_POINT('Ctrl Pts',(-1.89136993975585,-1.,-0.43522566096358));
#22725=CARTESIAN_POINT('Ctrl Pts',(-1.89663648956549,-1.,-0.437995003948443));
#22726=CARTESIAN_POINT('Ctrl Pts',(-1.90180124389137,-1.,-0.44080783370416));
#22727=CARTESIAN_POINT('Ctrl Pts',(-1.90691756144906,-1.,-0.44367755684917));
#22728=CARTESIAN_POINT('Ctrl Pts',(-1.91203699981095,-1.,-0.446617343485651));
#22729=CARTESIAN_POINT('Ctrl Pts',(-1.91718342555717,-1.,-0.449632260106572));
#22730=CARTESIAN_POINT('Ctrl Pts',(-1.9223538064847,-1.,-0.452719478359356));
#22731=CARTESIAN_POINT('Ctrl Pts',(-1.92753067150461,-1.,-0.455872005174335));
#22732=CARTESIAN_POINT('Ctrl Pts',(-1.93269066517936,-1.,-0.459081234547931));
#22733=CARTESIAN_POINT('Ctrl Pts',(-1.93781486640834,-1.,-0.462340031009087));
#22734=CARTESIAN_POINT('Ctrl Pts',(-1.94289794196205,-1.,-0.465645462026064));
#22735=CARTESIAN_POINT('Ctrl Pts',(-1.94794381136524,-1.,-0.468997482913158));
#22736=CARTESIAN_POINT('Ctrl Pts',(-1.95296148278136,-1.,-0.472397672264079));
#22737=CARTESIAN_POINT('Ctrl Pts',(-1.95796111148175,-1.,-0.475848034683171));
#22738=CARTESIAN_POINT('Ctrl Pts',(-1.96294933055938,-1.,-0.479349583074846));
#22739=CARTESIAN_POINT('Ctrl Pts',(-1.96792703422358,-1.,-0.482901662120686));
#22740=CARTESIAN_POINT('Ctrl Pts',(-1.97289186263272,-1.,-0.486502692907661));
#22741=CARTESIAN_POINT('Ctrl Pts',(-1.97783973019229,-1.,-0.490150627860955));
#22742=CARTESIAN_POINT('Ctrl Pts',(-1.9827665876182,-1.,-0.493843476541492));
#22743=CARTESIAN_POINT('Ctrl Pts',(-1.98767044752929,-1.,-0.497579909545564));
#22744=CARTESIAN_POINT('Ctrl Pts',(-1.9925514912615,-1.,-0.501359287727129));
#22745=CARTESIAN_POINT('Ctrl Pts',(-1.99741107463567,-1.,-0.505181361323011));
#22746=CARTESIAN_POINT('Ctrl Pts',(-2.00225107134733,-1.,-0.509046069886152));
#22747=CARTESIAN_POINT('Ctrl Pts',(-2.00707309946955,-1.,-0.512953306961813));
#22748=CARTESIAN_POINT('Ctrl Pts',(-2.01187773939257,-1.,-0.516902681728733));
#22749=CARTESIAN_POINT('Ctrl Pts',(-2.01666477917305,-1.,-0.520893590399428));
#22750=CARTESIAN_POINT('Ctrl Pts',(-2.02143356304712,-1.,-0.524925318333518));
#22751=CARTESIAN_POINT('Ctrl Pts',(-2.02618329083289,-1.,-0.52899712724191));
#22752=CARTESIAN_POINT('Ctrl Pts',(-2.03091336214401,-1.,-0.533108355132905));
#22753=CARTESIAN_POINT('Ctrl Pts',(-2.03562362953993,-1.,-0.537258489833134));
#22754=CARTESIAN_POINT('Ctrl Pts',(-2.0403142269048,-1.,-0.54144712061552));
#22755=CARTESIAN_POINT('Ctrl Pts',(-2.0449854471456,-1.,-0.545673903817348));
#22756=CARTESIAN_POINT('Ctrl Pts',(-2.04963761077974,-1.,-0.549938525150342));
#22757=CARTESIAN_POINT('Ctrl Pts',(-2.05427091604482,-1.,-0.554240657464109));
#22758=CARTESIAN_POINT('Ctrl Pts',(-2.05888537756571,-1.,-0.558579940185467));
#22759=CARTESIAN_POINT('Ctrl Pts',(-2.06348090160697,-1.,-0.562955993082574));
#22760=CARTESIAN_POINT('Ctrl Pts',(-2.06805732997383,-1.,-0.567368421181229));
#22761=CARTESIAN_POINT('Ctrl Pts',(-2.07261449292757,-1.,-0.571816823242411));
#22762=CARTESIAN_POINT('Ctrl Pts',(-2.07715226767361,-1.,-0.576300797416274));
#22763=CARTESIAN_POINT('Ctrl Pts',(-2.08167059018138,-1.,-0.580819952107257));
#22764=CARTESIAN_POINT('Ctrl Pts',(-2.086169437277,-1.,-0.585373918990895));
#22765=CARTESIAN_POINT('Ctrl Pts',(-2.09064881812053,-1.,-0.589962365403189));
#22766=CARTESIAN_POINT('Ctrl Pts',(-2.09510876220501,-1.,-0.594585006052823));
#22767=CARTESIAN_POINT('Ctrl Pts',(-2.09954930865331,-1.,-0.599241616422144));
#22768=CARTESIAN_POINT('Ctrl Pts',(-2.10397049887709,-1.,-0.603932030738212));
#22769=CARTESIAN_POINT('Ctrl Pts',(-2.10749199615859,-1.,-0.607711315456826));
#22770=CARTESIAN_POINT('Ctrl Pts',(-2.11012443807661,-1.,-0.610560911691113));
#22771=CARTESIAN_POINT('Ctrl Pts',(-2.11187554260142,-1.,-0.61246736556225));
#22772=CARTESIAN_POINT('Ctrl Pts',(-2.11275013067528,-1.,-0.61342227326009));
#22773=CARTESIAN_POINT('',(-2.0698113262342,-1.,-0.745574324794401));
#22774=CARTESIAN_POINT('',(-2.11275013067528,-1.,-0.61342227326009));
#22775=CARTESIAN_POINT('',(-1.60662857109684,-1.,-0.693717979106306));
#22776=CARTESIAN_POINT('Ctrl Pts',(-2.0698113262342,-1.,-0.745574324794401));
#22777=CARTESIAN_POINT('Ctrl Pts',(-2.06854248895575,-1.,-0.74583279137781));
#22778=CARTESIAN_POINT('Ctrl Pts',(-2.06600523016401,-1.,-0.746345871542695));
#22779=CARTESIAN_POINT('Ctrl Pts',(-2.06220058927162,-1.,-0.747103932785504));
#22780=CARTESIAN_POINT('Ctrl Pts',(-2.05713023030263,-1.,-0.748091554181101));
#22781=CARTESIAN_POINT('Ctrl Pts',(-2.05079645591606,-1.,-0.749287468663053));
#22782=CARTESIAN_POINT('Ctrl Pts',(-2.04446689147754,-1.,-0.750444657874758));
#22783=CARTESIAN_POINT('Ctrl Pts',(-2.03814160092173,-1.,-0.751562963361383));
#22784=CARTESIAN_POINT('Ctrl Pts',(-2.03182068456467,-1.,-0.752642180488104));
#22785=CARTESIAN_POINT('Ctrl Pts',(-2.02550428623587,-1.,-0.753682061113765));
#22786=CARTESIAN_POINT('Ctrl Pts',(-2.01919259406003,-1.,-0.75468233072352));
#22787=CARTESIAN_POINT('Ctrl Pts',(-2.01288584328149,-1.,-0.7556427049581));
#22788=CARTESIAN_POINT('Ctrl Pts',(-2.00658431587682,-1.,-0.756562904646496));
#22789=CARTESIAN_POINT('Ctrl Pts',(-2.00028834739072,-1.,-0.757442676862341));
#22790=CARTESIAN_POINT('Ctrl Pts',(-1.9939983109871,-1.,-0.758281796766377));
#22791=CARTESIAN_POINT('Ctrl Pts',(-1.98771456680806,-1.,-0.759080037802242));
#22792=CARTESIAN_POINT('Ctrl Pts',(-1.98143741418156,-1.,-0.759837147452135));
#22793=CARTESIAN_POINT('Ctrl Pts',(-1.97516705321521,-1.,-0.760552825409855));
#22794=CARTESIAN_POINT('Ctrl Pts',(-1.96890351582545,-1.,-0.761226690483986));
#22795=CARTESIAN_POINT('Ctrl Pts',(-1.96264672744229,-1.,-0.761858300014575));
#22796=CARTESIAN_POINT('Ctrl Pts',(-1.95639665309893,-1.,-0.762447203806263));
#22797=CARTESIAN_POINT('Ctrl Pts',(-1.95015342590025,-1.,-0.762992990878774));
#22798=CARTESIAN_POINT('Ctrl Pts',(-1.94391746617626,-1.,-0.76349533353858));
#22799=CARTESIAN_POINT('Ctrl Pts',(-1.93768964875867,-1.,-0.763954049121393));
#22800=CARTESIAN_POINT('Ctrl Pts',(-1.93147105496367,-1.,-0.764369010673889));
#22801=CARTESIAN_POINT('Ctrl Pts',(-1.92526263537041,-1.,-0.764740025488189));
#22802=CARTESIAN_POINT('Ctrl Pts',(-1.91906491634197,-1.,-0.765066729667095));
#22803=CARTESIAN_POINT('Ctrl Pts',(-1.91287765805174,-1.,-0.765348465884739));
#22804=CARTESIAN_POINT('Ctrl Pts',(-1.90669961402362,-1.,-0.765584196937936));
#22805=CARTESIAN_POINT('Ctrl Pts',(-1.90052930393599,-1.,-0.765772772593395));
#22806=CARTESIAN_POINT('Ctrl Pts',(-1.89436577771389,-1.,-0.765913193856979));
#22807=CARTESIAN_POINT('Ctrl Pts',(-1.88820926433409,-1.,-0.76600483706209));
#22808=CARTESIAN_POINT('Ctrl Pts',(-1.88206215302561,-1.,-0.766047794851868));
#22809=CARTESIAN_POINT('Ctrl Pts',(-1.87592888967886,-1.,-0.766042837036759));
#22810=CARTESIAN_POINT('Ctrl Pts',(-1.86981398314345,-1.,-0.765990708546111));
#22811=CARTESIAN_POINT('Ctrl Pts',(-1.86372027063314,-1.,-0.765891519092557));
#22812=CARTESIAN_POINT('Ctrl Pts',(-1.85764741390391,-1.,-0.765744212909305));
#22813=CARTESIAN_POINT('Ctrl Pts',(-1.85158945130054,-1.,-0.765545710619023));
#22814=CARTESIAN_POINT('Ctrl Pts',(-1.8455369887591,-1.,-0.765291664861971));
#22815=CARTESIAN_POINT('Ctrl Pts',(-1.83948181064823,-1.,-0.764978057881687));
#22816=CARTESIAN_POINT('Ctrl Pts',(-1.8334207722714,-1.,-0.764602549687845));
#22817=CARTESIAN_POINT('Ctrl Pts',(-1.8273599120008,-1.,-0.764165902606055));
#22818=CARTESIAN_POINT('Ctrl Pts',(-1.82131873145297,-1.,-0.763673465462854));
#22819=CARTESIAN_POINT('Ctrl Pts',(-1.81532118405566,-1.,-0.763132003836783));
#22820=CARTESIAN_POINT('Ctrl Pts',(-1.80938551463989,-1.,-0.762546129464036));
#22821=CARTESIAN_POINT('Ctrl Pts',(-1.80351583877334,-1.,-0.761915336443515));
#22822=CARTESIAN_POINT('Ctrl Pts',(-1.79768986997735,-1.,-0.761229695230359));
#22823=CARTESIAN_POINT('Ctrl Pts',(-1.79185815610802,-1.,-0.760469555880425));
#22824=CARTESIAN_POINT('Ctrl Pts',(-1.78596964884526,-1.,-0.759614401109868));
#22825=CARTESIAN_POINT('Ctrl Pts',(-1.77999411220912,-1.,-0.75865062667738));
#22826=CARTESIAN_POINT('Ctrl Pts',(-1.77394167108342,-1.,-0.757578264077238));
#22827=CARTESIAN_POINT('Ctrl Pts',(-1.76789396003141,-1.,-0.756421896028403));
#22828=CARTESIAN_POINT('Ctrl Pts',(-1.7619781724032,-1.,-0.755220979975262));
#22829=CARTESIAN_POINT('Ctrl Pts',(-1.75631083600175,-1.,-0.75400925402848));
#22830=CARTESIAN_POINT('Ctrl Pts',(-1.75095139468809,-1.,-0.752797683531377));
#22831=CARTESIAN_POINT('Ctrl Pts',(-1.74585086852298,-1.,-0.751555614163629));
#22832=CARTESIAN_POINT('Ctrl Pts',(-1.74080458266705,-1.,-0.75019343597954));
#22833=CARTESIAN_POINT('Ctrl Pts',(-1.73550351679848,-1.,-0.748582462954854));
#22834=CARTESIAN_POINT('Ctrl Pts',(-1.72958533647399,-1.,-0.746574710096436));
#22835=CARTESIAN_POINT('Ctrl Pts',(-1.7226822991693,-1.,-0.744021445433764));
#22836=CARTESIAN_POINT('Ctrl Pts',(-1.71447789751927,-1.,-0.740795162032087));
#22837=CARTESIAN_POINT('Ctrl Pts',(-1.70473309006121,-1.,-0.736799665724771));
#22838=CARTESIAN_POINT('Ctrl Pts',(-1.69326921975743,-1.,-0.731963238697195));
#22839=CARTESIAN_POINT('Ctrl Pts',(-1.67996158455503,-1.,-0.726235967997433));
#22840=CARTESIAN_POINT('Ctrl Pts',(-1.6647288055568,-1.,-0.719585433804282));
#22841=CARTESIAN_POINT('Ctrl Pts',(-1.64752408832016,-1.,-0.711993139355394));
#22842=CARTESIAN_POINT('Ctrl Pts',(-1.63216541664676,-1.,-0.705159151988319));
#22843=CARTESIAN_POINT('Ctrl Pts',(-1.61974673472612,-1.,-0.699605146405088));
#22844=CARTESIAN_POINT('Ctrl Pts',(-1.61106790958151,-1.,-0.695712097881194));
#22845=CARTESIAN_POINT('Ctrl Pts',(-1.60662857109684,-1.,-0.693717979106306));
#22846=CARTESIAN_POINT('',(-1.5055822144029,-1.,-0.892032620296855));
#22847=CARTESIAN_POINT('Origin',(0.,-1.,0.));
#22848=CARTESIAN_POINT('',(-1.81978687191668,-1.,-1.23627494547115));
#22849=CARTESIAN_POINT('Ctrl Pts',(-1.5055822144029,-1.,-0.892032620296855));
#22850=CARTESIAN_POINT('Ctrl Pts',(-1.50980486806688,-1.,-0.894452006964543));
#22851=CARTESIAN_POINT('Ctrl Pts',(-1.51805569590094,-1.,-0.899185047483511));
#22852=CARTESIAN_POINT('Ctrl Pts',(-1.52984849887993,-1.,-0.905967409625651));
#22853=CARTESIAN_POINT('Ctrl Pts',(-1.54440491149498,-1.,-0.914375919026456));
#22854=CARTESIAN_POINT('Ctrl Pts',(-1.56065988578893,-1.,-0.923832188944341));
#22855=CARTESIAN_POINT('Ctrl Pts',(-1.57499388382243,-1.,-0.932246680108685));
#22856=CARTESIAN_POINT('Ctrl Pts',(-1.58744937487176,-1.,-0.939646377893399));
#22857=CARTESIAN_POINT('Ctrl Pts',(-1.59810042043673,-1.,-0.946078063315257));
#22858=CARTESIAN_POINT('Ctrl Pts',(-1.60706069896936,-1.,-0.951613284356035));
#22859=CARTESIAN_POINT('Ctrl Pts',(-1.61449324337085,-1.,-0.956354422920671));
#22860=CARTESIAN_POINT('Ctrl Pts',(-1.62061638140221,-1.,-0.960438326101729));
#22861=CARTESIAN_POINT('Ctrl Pts',(-1.62571930670187,-1.,-0.964046107040536));
#22862=CARTESIAN_POINT('Ctrl Pts',(-1.63013849959461,-1.,-0.967387853230345));
#22863=CARTESIAN_POINT('Ctrl Pts',(-1.63420665729798,-1.,-0.970669715997509));
#22864=CARTESIAN_POINT('Ctrl Pts',(-1.63820952658144,-1.,-0.974066058287418));
#22865=CARTESIAN_POINT('Ctrl Pts',(-1.64233990826687,-1.,-0.977689794119416));
#22866=CARTESIAN_POINT('Ctrl Pts',(-1.64665139190656,-1.,-0.981562530939489));
#22867=CARTESIAN_POINT('Ctrl Pts',(-1.65110016612638,-1.,-0.985642622920821));
#22868=CARTESIAN_POINT('Ctrl Pts',(-1.65559044289699,-1.,-0.989855627854165));
#22869=CARTESIAN_POINT('Ctrl Pts',(-1.66001553809947,-1.,-0.994121836661306));
#22870=CARTESIAN_POINT('Ctrl Pts',(-1.66430758030376,-1.,-0.998389654952758));
#22871=CARTESIAN_POINT('Ctrl Pts',(-1.66846059277303,-1.,-1.00265091003727));
#22872=CARTESIAN_POINT('Ctrl Pts',(-1.67250335383293,-1.,-1.00692206696414));
#22873=CARTESIAN_POINT('Ctrl Pts',(-1.67648246776464,-1.,-1.01123236493511));
#22874=CARTESIAN_POINT('Ctrl Pts',(-1.68044289894798,-1.,-1.01561026162773));
#22875=CARTESIAN_POINT('Ctrl Pts',(-1.68440578021706,-1.,-1.02006795074201));
#22876=CARTESIAN_POINT('Ctrl Pts',(-1.68836910178447,-1.,-1.02460180535255));
#22877=CARTESIAN_POINT('Ctrl Pts',(-1.69231840863458,-1.,-1.02919977579147));
#22878=CARTESIAN_POINT('Ctrl Pts',(-1.69623414782771,-1.,-1.03384646003588));
#22879=CARTESIAN_POINT('Ctrl Pts',(-1.70010052930962,-1.,-1.03852922490789));
#22880=CARTESIAN_POINT('Ctrl Pts',(-1.70391338707982,-1.,-1.04324363334554));
#22881=CARTESIAN_POINT('Ctrl Pts',(-1.70767646263649,-1.,-1.04799085404995));
#22882=CARTESIAN_POINT('Ctrl Pts',(-1.71139783543989,-1.,-1.05277517202855));
#22883=CARTESIAN_POINT('Ctrl Pts',(-1.7150865442702,-1.,-1.05760163192479));
#22884=CARTESIAN_POINT('Ctrl Pts',(-1.71874858456904,-1.,-1.06247324680647));
#22885=CARTESIAN_POINT('Ctrl Pts',(-1.72238500928453,-1.,-1.06738966975462));
#22886=CARTESIAN_POINT('Ctrl Pts',(-1.72599406198488,-1.,-1.07234866990252));
#22887=CARTESIAN_POINT('Ctrl Pts',(-1.72957248977424,-1.,-1.0773470373727));
#22888=CARTESIAN_POINT('Ctrl Pts',(-1.73311705663407,-1.,-1.08238162784749));
#22889=CARTESIAN_POINT('Ctrl Pts',(-1.73662628326091,-1.,-1.08745056285427));
#22890=CARTESIAN_POINT('Ctrl Pts',(-1.74010053962247,-1.,-1.09255329056493));
#22891=CARTESIAN_POINT('Ctrl Pts',(-1.74354119236208,-1.,-1.09768999241225));
#22892=CARTESIAN_POINT('Ctrl Pts',(-1.74695004214923,-1.,-1.10286118991143));
#22893=CARTESIAN_POINT('Ctrl Pts',(-1.7503286607592,-1.,-1.10806728183007));
#22894=CARTESIAN_POINT('Ctrl Pts',(-1.7536777209463,-1.,-1.11330807582551));
#22895=CARTESIAN_POINT('Ctrl Pts',(-1.75699720772105,-1.,-1.11858293216763));
#22896=CARTESIAN_POINT('Ctrl Pts',(-1.76028671825096,-1.,-1.12389096855086));
#22897=CARTESIAN_POINT('Ctrl Pts',(-1.7635457196617,-1.,-1.12923123555075));
#22898=CARTESIAN_POINT('Ctrl Pts',(-1.76677384551862,-1.,-1.1346029180462));
#22899=CARTESIAN_POINT('Ctrl Pts',(-1.76997111386769,-1.,-1.14000548336975));
#22900=CARTESIAN_POINT('Ctrl Pts',(-1.77313777896194,-1.,-1.1454385822692));
#22901=CARTESIAN_POINT('Ctrl Pts',(-1.7762742255701,-1.,-1.15090197841515));
#22902=CARTESIAN_POINT('Ctrl Pts',(-1.77938085564275,-1.,-1.15639547194698));
#22903=CARTESIAN_POINT('Ctrl Pts',(-1.78245795881009,-1.,-1.16191881298499));
#22904=CARTESIAN_POINT('Ctrl Pts',(-1.78550566040443,-1.,-1.16747166312303));
#22905=CARTESIAN_POINT('Ctrl Pts',(-1.78852398877616,-1.,-1.17305363177328));
#22906=CARTESIAN_POINT('Ctrl Pts',(-1.79151291552689,-1.,-1.17866429440809));
#22907=CARTESIAN_POINT('Ctrl Pts',(-1.79447240321515,-1.,-1.18430321697432));
#22908=CARTESIAN_POINT('Ctrl Pts',(-1.79740245923478,-1.,-1.18996997934445));
#22909=CARTESIAN_POINT('Ctrl Pts',(-1.80030314369879,-1.,-1.19566418930242));
#22910=CARTESIAN_POINT('Ctrl Pts',(-1.80317454838603,-1.,-1.20138548938974));
#22911=CARTESIAN_POINT('Ctrl Pts',(-1.80601678480707,-1.,-1.20713356605475));
#22912=CARTESIAN_POINT('Ctrl Pts',(-1.80882996917129,-1.,-1.21290815708314));
#22913=CARTESIAN_POINT('Ctrl Pts',(-1.81161420806656,-1.,-1.21870906103557));
#22914=CARTESIAN_POINT('Ctrl Pts',(-1.81436959210434,-1.,-1.2245361330495));
#22915=CARTESIAN_POINT('Ctrl Pts',(-1.8165508718364,-1.,-1.2292186489137));
#22916=CARTESIAN_POINT('Ctrl Pts',(-1.81817389921279,-1.,-1.2327422452705));
#22917=CARTESIAN_POINT('Ctrl Pts',(-1.81925017193666,-1.,-1.23509651170476));
#22918=CARTESIAN_POINT('Ctrl Pts',(-1.81978687191668,-1.,-1.23627494547115));
#22919=CARTESIAN_POINT('',(-1.73811241238545,-1.,-1.34869019493419));
#22920=CARTESIAN_POINT('',(-1.81978687191668,-1.,-1.23627494547115));
#22921=CARTESIAN_POINT('',(-1.31362392696032,-1.,-1.15624053661742));
#22922=CARTESIAN_POINT('Ctrl Pts',(-1.73811241238545,-1.,-1.34869019493419));
#22923=CARTESIAN_POINT('Ctrl Pts',(-1.73682580585691,-1.,-1.34854391898045));
#22924=CARTESIAN_POINT('Ctrl Pts',(-1.73425417885907,-1.,-1.34824783112887));
#22925=CARTESIAN_POINT('Ctrl Pts',(-1.7304014965394,-1.,-1.34779309152035));
#22926=CARTESIAN_POINT('Ctrl Pts',(-1.72527410680674,-1.,-1.34716554819527));
#22927=CARTESIAN_POINT('Ctrl Pts',(-1.7188807715049,-1.,-1.34634568653227));
#22928=CARTESIAN_POINT('Ctrl Pts',(-1.71250340686822,-1.,-1.34549029589416));
#22929=CARTESIAN_POINT('Ctrl Pts',(-1.70614212266738,-1.,-1.34459924533831));
#22930=CARTESIAN_POINT('Ctrl Pts',(-1.69979707754427,-1.,-1.34367237124483));
#22931=CARTESIAN_POINT('Ctrl Pts',(-1.6934684849687,-1.,-1.34270948206319));
#22932=CARTESIAN_POINT('Ctrl Pts',(-1.68715660868764,-1.,-1.341710374848));
#22933=CARTESIAN_POINT('Ctrl Pts',(-1.68086176030362,-1.,-1.34067485185203));
#22934=CARTESIAN_POINT('Ctrl Pts',(-1.67458429426086,-1.,-1.3396027347034));
#22935=CARTESIAN_POINT('Ctrl Pts',(-1.66832460783989,-1.,-1.33849388654388));
#22936=CARTESIAN_POINT('Ctrl Pts',(-1.66208312541983,-1.,-1.33734820885262));
#22937=CARTESIAN_POINT('Ctrl Pts',(-1.65586025952593,-1.,-1.33616559745172));
#22938=CARTESIAN_POINT('Ctrl Pts',(-1.6496563728683,-1.,-1.33494590467993));
#22939=CARTESIAN_POINT('Ctrl Pts',(-1.6434717485603,-1.,-1.33368890676572));
#22940=CARTESIAN_POINT('Ctrl Pts',(-1.63730653475089,-1.,-1.33239425103724));
#22941=CARTESIAN_POINT('Ctrl Pts',(-1.63116079730923,-1.,-1.33106149345645));
#22942=CARTESIAN_POINT('Ctrl Pts',(-1.62503464209797,-1.,-1.3296901950568));
#22943=CARTESIAN_POINT('Ctrl Pts',(-1.61892832270724,-1.,-1.32828000610449));
#22944=CARTESIAN_POINT('Ctrl Pts',(-1.6128423401575,-1.,-1.32683074483356));
#22945=CARTESIAN_POINT('Ctrl Pts',(-1.60677758290954,-1.,-1.32534250785782));
#22946=CARTESIAN_POINT('Ctrl Pts',(-1.60073511858687,-1.,-1.32381550858256));
#22947=CARTESIAN_POINT('Ctrl Pts',(-1.59471591079403,-1.,-1.32224985747682));
#22948=CARTESIAN_POINT('Ctrl Pts',(-1.58872057258245,-1.,-1.32064537110892));
#22949=CARTESIAN_POINT('Ctrl Pts',(-1.58274907898834,-1.,-1.31900135021432));
#22950=CARTESIAN_POINT('Ctrl Pts',(-1.5768005650559,-1.,-1.31731642317187));
#22951=CARTESIAN_POINT('Ctrl Pts',(-1.57087397835723,-1.,-1.31558903860016));
#22952=CARTESIAN_POINT('Ctrl Pts',(-1.56496872402353,-1.,-1.31381795281002));
#22953=CARTESIAN_POINT('Ctrl Pts',(-1.55908521254821,-1.,-1.31200264341696));
#22954=CARTESIAN_POINT('Ctrl Pts',(-1.55322568759481,-1.,-1.31014393684222));
#22955=CARTESIAN_POINT('Ctrl Pts',(-1.54739413957185,-1.,-1.30824393907473));
#22956=CARTESIAN_POINT('Ctrl Pts',(-1.54159462645432,-1.,-1.30630475189556));
#22957=CARTESIAN_POINT('Ctrl Pts',(-1.53582981268977,-1.,-1.30432735639489));
#22958=CARTESIAN_POINT('Ctrl Pts',(-1.53009970283891,-1.,-1.30231064395568));
#22959=CARTESIAN_POINT('Ctrl Pts',(-1.52439957861062,-1.,-1.30024984366328));
#22960=CARTESIAN_POINT('Ctrl Pts',(-1.51872184912724,-1.,-1.29813791800747));
#22961=CARTESIAN_POINT('Ctrl Pts',(-1.51305994241402,-1.,-1.29596850710509));
#22962=CARTESIAN_POINT('Ctrl Pts',(-1.50741159078365,-1.,-1.29373841372842));
#22963=CARTESIAN_POINT('Ctrl Pts',(-1.50178230149776,-1.,-1.29145022885181));
#22964=CARTESIAN_POINT('Ctrl Pts',(-1.49618896881754,-1.,-1.28911506584254));
#22965=CARTESIAN_POINT('Ctrl Pts',(-1.4906522831278,-1.,-1.2867467611644));
#22966=CARTESIAN_POINT('Ctrl Pts',(-1.4851881711891,-1.,-1.28435533880201));
#22967=CARTESIAN_POINT('Ctrl Pts',(-1.47980070347095,-1.,-1.28194158939517));
#22968=CARTESIAN_POINT('Ctrl Pts',(-1.4744717526707,-1.,-1.2794891824849));
#22969=CARTESIAN_POINT('Ctrl Pts',(-1.46916035917133,-1.,-1.27696414831089));
#22970=CARTESIAN_POINT('Ctrl Pts',(-1.46382431332476,-1.,-1.27433119897822));
#22971=CARTESIAN_POINT('Ctrl Pts',(-1.45843906294697,-1.,-1.27156805265289));
#22972=CARTESIAN_POINT('Ctrl Pts',(-1.45301422764247,-1.,-1.2686778680489));
#22973=CARTESIAN_POINT('Ctrl Pts',(-1.44761985001662,-1.,-1.26570925118868));
#22974=CARTESIAN_POINT('Ctrl Pts',(-1.44236470511303,-1.,-1.26273903323859));
#22975=CARTESIAN_POINT('Ctrl Pts',(-1.43734919180848,-1.,-1.25983531012005));
#22976=CARTESIAN_POINT('Ctrl Pts',(-1.43262645609691,-1.,-1.25702687965755));
#22977=CARTESIAN_POINT('Ctrl Pts',(-1.42815938799387,-1.,-1.25426945222639));
#22978=CARTESIAN_POINT('Ctrl Pts',(-1.42378102115575,-1.,-1.2514145557001));
#22979=CARTESIAN_POINT('Ctrl Pts',(-1.41923722596025,-1.,-1.24824430986571));
#22980=CARTESIAN_POINT('Ctrl Pts',(-1.41422913175179,-1.,-1.24450600513056));
#22981=CARTESIAN_POINT('Ctrl Pts',(-1.40845295531283,-1.,-1.23994455029534));
#22982=CARTESIAN_POINT('Ctrl Pts',(-1.40164708206106,-1.,-1.23434087290423));
#22983=CARTESIAN_POINT('Ctrl Pts',(-1.39361389568796,-1.,-1.22752961899387));
#22984=CARTESIAN_POINT('Ctrl Pts',(-1.38420564527715,-1.,-1.21938737280852));
#22985=CARTESIAN_POINT('Ctrl Pts',(-1.37331915607905,-1.,-1.20982812925645));
#22986=CARTESIAN_POINT('Ctrl Pts',(-1.36088705043885,-1.,-1.1987959077932));
#22987=CARTESIAN_POINT('Ctrl Pts',(-1.34687054001093,-1.,-1.18625865667441));
#22988=CARTESIAN_POINT('Ctrl Pts',(-1.33437539347008,-1.,-1.17501305789857));
#22989=CARTESIAN_POINT('Ctrl Pts',(-1.32428080721772,-1.,-1.16589330093588));
#22990=CARTESIAN_POINT('Ctrl Pts',(-1.31722977216397,-1.,-1.15950888730809));
#22991=CARTESIAN_POINT('Ctrl Pts',(-1.31362392696032,-1.,-1.15624053661742));
#22992=CARTESIAN_POINT('',(-1.15624053661742,-1.,-1.31362392696033));
#22993=CARTESIAN_POINT('Origin',(0.,-1.,0.));
#22994=CARTESIAN_POINT('',(-1.34869019493419,-1.,-1.73811241238545));
#22995=CARTESIAN_POINT('Ctrl Pts',(-1.15624053661742,-1.,-1.31362392696033));
#22996=CARTESIAN_POINT('Ctrl Pts',(-1.15950888730433,-1.,-1.3172297721596));
#22997=CARTESIAN_POINT('Ctrl Pts',(-1.16589330092532,-1.,-1.32428080720544));
#22998=CARTESIAN_POINT('Ctrl Pts',(-1.17501305787994,-1.,-1.33437539344842));
#22999=CARTESIAN_POINT('Ctrl Pts',(-1.18625865664915,-1.,-1.34687053998157));
#23000=CARTESIAN_POINT('Ctrl Pts',(-1.1987959077656,-1.,-1.36088705040677));
#23001=CARTESIAN_POINT('Ctrl Pts',(-1.20982812923113,-1.,-1.37331915604962));
#23002=CARTESIAN_POINT('Ctrl Pts',(-1.21938737278853,-1.,-1.38420564525391));
#23003=CARTESIAN_POINT('Ctrl Pts',(-1.22752961898063,-1.,-1.39361389567257));
#23004=CARTESIAN_POINT('Ctrl Pts',(-1.23434087289768,-1.,-1.40164708205345));
#23005=CARTESIAN_POINT('Ctrl Pts',(-1.23994455029421,-1.,-1.40845295531151));
#23006=CARTESIAN_POINT('Ctrl Pts',(-1.24450600513278,-1.,-1.41422913175437));
#23007=CARTESIAN_POINT('Ctrl Pts',(-1.24824430986911,-1.,-1.41923722596421));
#23008=CARTESIAN_POINT('Ctrl Pts',(-1.25141455570299,-1.,-1.42378102115911));
#23009=CARTESIAN_POINT('Ctrl Pts',(-1.25426945222783,-1.,-1.42815938799555));
#23010=CARTESIAN_POINT('Ctrl Pts',(-1.25702687965744,-1.,-1.43262645609679));
#23011=CARTESIAN_POINT('Ctrl Pts',(-1.25983531011894,-1.,-1.43734919180719));
#23012=CARTESIAN_POINT('Ctrl Pts',(-1.26273903323723,-1.,-1.44236470511145));
#23013=CARTESIAN_POINT('Ctrl Pts',(-1.26570925118767,-1.,-1.44761985001544));
#23014=CARTESIAN_POINT('Ctrl Pts',(-1.26867786804854,-1.,-1.45301422764205));
#23015=CARTESIAN_POINT('Ctrl Pts',(-1.27156805265312,-1.,-1.45843906294725));
#23016=CARTESIAN_POINT('Ctrl Pts',(-1.27433119897877,-1.,-1.4638243133254));
#23017=CARTESIAN_POINT('Ctrl Pts',(-1.27696414831144,-1.,-1.46916035917197));
#23018=CARTESIAN_POINT('Ctrl Pts',(-1.27948918248524,-1.,-1.4744717526711));
#23019=CARTESIAN_POINT('Ctrl Pts',(-1.28194158939522,-1.,-1.47980070347102));
#23020=CARTESIAN_POINT('Ctrl Pts',(-1.28435533880184,-1.,-1.48518817118891));
#23021=CARTESIAN_POINT('Ctrl Pts',(-1.28674676116415,-1.,-1.4906522831275));
#23022=CARTESIAN_POINT('Ctrl Pts',(-1.28911506584232,-1.,-1.49618896881729));
#23023=CARTESIAN_POINT('Ctrl Pts',(-1.29145022885171,-1.,-1.50178230149764));
#23024=CARTESIAN_POINT('Ctrl Pts',(-1.29373841372843,-1.,-1.50741159078367));
#23025=CARTESIAN_POINT('Ctrl Pts',(-1.29596850710518,-1.,-1.51305994241412));
#23026=CARTESIAN_POINT('Ctrl Pts',(-1.29813791800757,-1.,-1.51872184912735));
#23027=CARTESIAN_POINT('Ctrl Pts',(-1.30024984366334,-1.,-1.5243995786107));
#23028=CARTESIAN_POINT('Ctrl Pts',(-1.3023106439557,-1.,-1.53009970283893));
#23029=CARTESIAN_POINT('Ctrl Pts',(-1.30432735639487,-1.,-1.53582981268976));
#23030=CARTESIAN_POINT('Ctrl Pts',(-1.30630475189553,-1.,-1.54159462645428));
#23031=CARTESIAN_POINT('Ctrl Pts',(-1.30824393907471,-1.,-1.54739413957183));
#23032=CARTESIAN_POINT('Ctrl Pts',(-1.31014393684221,-1.,-1.55322568759481));
#23033=CARTESIAN_POINT('Ctrl Pts',(-1.31200264341696,-1.,-1.55908521254822));
#23034=CARTESIAN_POINT('Ctrl Pts',(-1.31381795281002,-1.,-1.56496872402352));
#23035=CARTESIAN_POINT('Ctrl Pts',(-1.31558903860015,-1.,-1.57087397835721));
#23036=CARTESIAN_POINT('Ctrl Pts',(-1.31731642317183,-1.,-1.57680056505585));
#23037=CARTESIAN_POINT('Ctrl Pts',(-1.31900135021428,-1.,-1.58274907898829));
#23038=CARTESIAN_POINT('Ctrl Pts',(-1.32064537110891,-1.,-1.58872057258244));
#23039=CARTESIAN_POINT('Ctrl Pts',(-1.32224985747686,-1.,-1.59471591079408));
#23040=CARTESIAN_POINT('Ctrl Pts',(-1.32381550858266,-1.,-1.600735118587));
#23041=CARTESIAN_POINT('Ctrl Pts',(-1.32534250785794,-1.,-1.6067775829097));
#23042=CARTESIAN_POINT('Ctrl Pts',(-1.32683074483365,-1.,-1.61284234015762));
#23043=CARTESIAN_POINT('Ctrl Pts',(-1.32828000610448,-1.,-1.61892832270723));
#23044=CARTESIAN_POINT('Ctrl Pts',(-1.32969019505665,-1.,-1.62503464209777));
#23045=CARTESIAN_POINT('Ctrl Pts',(-1.33106149345618,-1.,-1.63116079730887));
#23046=CARTESIAN_POINT('Ctrl Pts',(-1.33239425103694,-1.,-1.6373065347505));
#23047=CARTESIAN_POINT('Ctrl Pts',(-1.33368890676554,-1.,-1.64347174856007));
#23048=CARTESIAN_POINT('Ctrl Pts',(-1.33494590468003,-1.,-1.64965637286843));
#23049=CARTESIAN_POINT('Ctrl Pts',(-1.33616559745217,-1.,-1.65586025952651));
#23050=CARTESIAN_POINT('Ctrl Pts',(-1.33734820885331,-1.,-1.66208312542073));
#23051=CARTESIAN_POINT('Ctrl Pts',(-1.33849388654458,-1.,-1.66832460784078));
#23052=CARTESIAN_POINT('Ctrl Pts',(-1.33960273470372,-1.,-1.67458429426126));
#23053=CARTESIAN_POINT('Ctrl Pts',(-1.3406748518516,-1.,-1.68086176030308));
#23054=CARTESIAN_POINT('Ctrl Pts',(-1.34171037484673,-1.,-1.68715660868602));
#23055=CARTESIAN_POINT('Ctrl Pts',(-1.34270948206139,-1.,-1.6934684849664));
#23056=CARTESIAN_POINT('Ctrl Pts',(-1.34367237124322,-1.,-1.69979707754221));
#23057=CARTESIAN_POINT('Ctrl Pts',(-1.34459924533783,-1.,-1.70614212266676));
#23058=CARTESIAN_POINT('Ctrl Pts',(-1.34549029589563,-1.,-1.71250340687011));
#23059=CARTESIAN_POINT('Ctrl Pts',(-1.34634568653586,-1.,-1.7188807715095));
#23060=CARTESIAN_POINT('Ctrl Pts',(-1.34716554820013,-1.,-1.72527410681298));
#23061=CARTESIAN_POINT('Ctrl Pts',(-1.3477930915247,-1.,-1.73040149654497));
#23062=CARTESIAN_POINT('Ctrl Pts',(-1.34824783113158,-1.,-1.73425417886255));
#23063=CARTESIAN_POINT('Ctrl Pts',(-1.34854391898145,-1.,-1.73682580585819));
#23064=CARTESIAN_POINT('Ctrl Pts',(-1.34869019493419,-1.,-1.73811241238545));
#23065=CARTESIAN_POINT('',(-1.23627494547115,-1.,-1.81978687191668));
#23066=CARTESIAN_POINT('',(-1.34869019493419,-1.,-1.73811241238545));
#23067=CARTESIAN_POINT('',(-0.892032620296855,-1.,-1.5055822144029));
#23068=CARTESIAN_POINT('Ctrl Pts',(-1.23627494547115,-1.,-1.81978687191668));
#23069=CARTESIAN_POINT('Ctrl Pts',(-1.23509651170384,-1.,-1.81925017193531));
#23070=CARTESIAN_POINT('Ctrl Pts',(-1.23274224526804,-1.,-1.81817389920914));
#23071=CARTESIAN_POINT('Ctrl Pts',(-1.22921864890975,-1.,-1.81655087183054));
#23072=CARTESIAN_POINT('Ctrl Pts',(-1.22453613304507,-1.,-1.81436959209778));
#23073=CARTESIAN_POINT('Ctrl Pts',(-1.2187090610323,-1.,-1.81161420806172));
#23074=CARTESIAN_POINT('Ctrl Pts',(-1.2129081570818,-1.,-1.80882996916931));
#23075=CARTESIAN_POINT('Ctrl Pts',(-1.20713356605519,-1.,-1.80601678480772));
#23076=CARTESIAN_POINT('Ctrl Pts',(-1.2013854893912,-1.,-1.8031745483882));
#23077=CARTESIAN_POINT('Ctrl Pts',(-1.19566418930405,-1.,-1.80030314370121));
#23078=CARTESIAN_POINT('Ctrl Pts',(-1.1899699793456,-1.,-1.79740245923649));
#23079=CARTESIAN_POINT('Ctrl Pts',(-1.18430321697471,-1.,-1.79447240321572));
#23080=CARTESIAN_POINT('Ctrl Pts',(-1.17866429440781,-1.,-1.79151291552646));
#23081=CARTESIAN_POINT('Ctrl Pts',(-1.17305363177265,-1.,-1.78852398877523));
#23082=CARTESIAN_POINT('Ctrl Pts',(-1.16747166312239,-1.,-1.78550566040349));
#23083=CARTESIAN_POINT('Ctrl Pts',(-1.16191881298458,-1.,-1.78245795880949));
#23084=CARTESIAN_POINT('Ctrl Pts',(-1.15639547194689,-1.,-1.77938085564261));
#23085=CARTESIAN_POINT('Ctrl Pts',(-1.15090197841531,-1.,-1.77627422557034));
#23086=CARTESIAN_POINT('Ctrl Pts',(-1.14543858226948,-1.,-1.77313777896234));
#23087=CARTESIAN_POINT('Ctrl Pts',(-1.14000548337,-1.,-1.76997111386806));
#23088=CARTESIAN_POINT('Ctrl Pts',(-1.13460291804635,-1.,-1.76677384551883));
#23089=CARTESIAN_POINT('Ctrl Pts',(-1.12923123555076,-1.,-1.76354571966171));
#23090=CARTESIAN_POINT('Ctrl Pts',(-1.12389096855078,-1.,-1.76028671825084));
#23091=CARTESIAN_POINT('Ctrl Pts',(-1.11858293216752,-1.,-1.75699720772089));
#23092=CARTESIAN_POINT('Ctrl Pts',(-1.11330807582542,-1.,-1.75367772094617));
#23093=CARTESIAN_POINT('Ctrl Pts',(-1.10806728183003,-1.,-1.75032866075914));
#23094=CARTESIAN_POINT('Ctrl Pts',(-1.10286118991144,-1.,-1.74695004214924));
#23095=CARTESIAN_POINT('Ctrl Pts',(-1.09768999241229,-1.,-1.74354119236212));
#23096=CARTESIAN_POINT('Ctrl Pts',(-1.09255329056496,-1.,-1.74010053962252));
#23097=CARTESIAN_POINT('Ctrl Pts',(-1.08745056285429,-1.,-1.73662628326093));
#23098=CARTESIAN_POINT('Ctrl Pts',(-1.08238162784749,-1.,-1.73311705663407));
#23099=CARTESIAN_POINT('Ctrl Pts',(-1.0773470373727,-1.,-1.72957248977424));
#23100=CARTESIAN_POINT('Ctrl Pts',(-1.07234866990252,-1.,-1.72599406198489));
#23101=CARTESIAN_POINT('Ctrl Pts',(-1.06738966975463,-1.,-1.72238500928456));
#23102=CARTESIAN_POINT('Ctrl Pts',(-1.0624732468065,-1.,-1.71874858456908));
#23103=CARTESIAN_POINT('Ctrl Pts',(-1.05760163192481,-1.,-1.71508654427022));
#23104=CARTESIAN_POINT('Ctrl Pts',(-1.05277517202854,-1.,-1.71139783543986));
#23105=CARTESIAN_POINT('Ctrl Pts',(-1.0479908540499,-1.,-1.70767646263641));
#23106=CARTESIAN_POINT('Ctrl Pts',(-1.04324363334546,-1.,-1.70391338707969));
#23107=CARTESIAN_POINT('Ctrl Pts',(-1.03852922490782,-1.,-1.70010052930951));
#23108=CARTESIAN_POINT('Ctrl Pts',(-1.03384646003587,-1.,-1.69623414782769));
#23109=CARTESIAN_POINT('Ctrl Pts',(-1.02919977579155,-1.,-1.69231840863471));
#23110=CARTESIAN_POINT('Ctrl Pts',(-1.02460180535272,-1.,-1.68836910178475));
#23111=CARTESIAN_POINT('Ctrl Pts',(-1.02006795074222,-1.,-1.68440578021739));
#23112=CARTESIAN_POINT('Ctrl Pts',(-1.01561026162787,-1.,-1.6804428989482));
#23113=CARTESIAN_POINT('Ctrl Pts',(-1.01123236493507,-1.,-1.67648246776457));
#23114=CARTESIAN_POINT('Ctrl Pts',(-1.00692206696387,-1.,-1.67250335383248));
#23115=CARTESIAN_POINT('Ctrl Pts',(-1.00265091003682,-1.,-1.66846059277231));
#23116=CARTESIAN_POINT('Ctrl Pts',(-0.998389654952317,-1.,-1.66430758030304));
#23117=CARTESIAN_POINT('Ctrl Pts',(-0.994121836661116,-1.,-1.66001553809916));
#23118=CARTESIAN_POINT('Ctrl Pts',(-0.98985562785445,-1.,-1.65559044289746));
#23119=CARTESIAN_POINT('Ctrl Pts',(-0.985642622921626,-1.,-1.6511001661277));
#23120=CARTESIAN_POINT('Ctrl Pts',(-0.981562530940574,-1.,-1.64665139190834));
#23121=CARTESIAN_POINT('Ctrl Pts',(-0.977689794120297,-1.,-1.64233990826831));
#23122=CARTESIAN_POINT('Ctrl Pts',(-0.974066058287501,-1.,-1.63820952658157));
#23123=CARTESIAN_POINT('Ctrl Pts',(-0.970669715996356,-1.,-1.63420665729609));
#23124=CARTESIAN_POINT('Ctrl Pts',(-0.967387853228041,-1.,-1.63013849959083));
#23125=CARTESIAN_POINT('Ctrl Pts',(-0.964046107037821,-1.,-1.6257193066974));
#23126=CARTESIAN_POINT('Ctrl Pts',(-0.960438326099958,-1.,-1.62061638139929));
#23127=CARTESIAN_POINT('Ctrl Pts',(-0.956354422921573,-1.,-1.61449324337233));
#23128=CARTESIAN_POINT('Ctrl Pts',(-0.951613284361248,-1.,-1.60706069897794));
#23129=CARTESIAN_POINT('Ctrl Pts',(-0.946078063325796,-1.,-1.59810042045408));
#23130=CARTESIAN_POINT('Ctrl Pts',(-0.939646377909319,-1.,-1.58744937489796));
#23131=CARTESIAN_POINT('Ctrl Pts',(-0.932246680128849,-1.,-1.57499388385561));
#23132=CARTESIAN_POINT('Ctrl Pts',(-0.923832188966322,-1.,-1.56065988582509));
#23133=CARTESIAN_POINT('Ctrl Pts',(-0.91437591904658,-1.,-1.54440491152808));
#23134=CARTESIAN_POINT('Ctrl Pts',(-0.905967409640499,-1.,-1.52984849890434));
#23135=CARTESIAN_POINT('Ctrl Pts',(-0.89918504749193,-1.,-1.51805569591479));
#23136=CARTESIAN_POINT('Ctrl Pts',(-0.894452006967538,-1.,-1.50980486807181));
#23137=CARTESIAN_POINT('Ctrl Pts',(-0.892032620296855,-1.,-1.5055822144029));
#23138=CARTESIAN_POINT('',(-0.693717979106305,-1.,-1.60662857109684));
#23139=CARTESIAN_POINT('Origin',(0.,-1.,0.));
#23140=CARTESIAN_POINT('',(-0.745574324794401,-1.,-2.0698113262342));
#23141=CARTESIAN_POINT('Ctrl Pts',(-0.693717979106305,-1.,-1.60662857109684));
#23142=CARTESIAN_POINT('Ctrl Pts',(-0.69571209787897,-1.,-1.61106790957619));
#23143=CARTESIAN_POINT('Ctrl Pts',(-0.699605146398837,-1.,-1.61974673471117));
#23144=CARTESIAN_POINT('Ctrl Pts',(-0.705159151977294,-1.,-1.6321654166204));
#23145=CARTESIAN_POINT('Ctrl Pts',(-0.711993139340447,-1.,-1.64752408828442));
#23146=CARTESIAN_POINT('Ctrl Pts',(-0.71958543378795,-1.,-1.66472880551777));
#23147=CARTESIAN_POINT('Ctrl Pts',(-0.726235967982445,-1.,-1.67996158451922));
#23148=CARTESIAN_POINT('Ctrl Pts',(-0.731963238685357,-1.,-1.69326921972915));
#23149=CARTESIAN_POINT('Ctrl Pts',(-0.736799665716932,-1.,-1.70473309004249));
#23150=CARTESIAN_POINT('Ctrl Pts',(-0.74079516202821,-1.,-1.71447789751001));
#23151=CARTESIAN_POINT('Ctrl Pts',(-0.744021445433093,-1.,-1.72268229916769));
#23152=CARTESIAN_POINT('Ctrl Pts',(-0.746574710097752,-1.,-1.72958533647714));
#23153=CARTESIAN_POINT('Ctrl Pts',(-0.74858246295687,-1.,-1.7355035168033));
#23154=CARTESIAN_POINT('Ctrl Pts',(-0.750193435981249,-1.,-1.74080458267114));
#23155=CARTESIAN_POINT('Ctrl Pts',(-0.751555614164482,-1.,-1.74585086852502));
#23156=CARTESIAN_POINT('Ctrl Pts',(-0.752797683531314,-1.,-1.75095139468794));
#23157=CARTESIAN_POINT('Ctrl Pts',(-0.754009254027829,-1.,-1.75631083600019));
#23158=CARTESIAN_POINT('Ctrl Pts',(-0.755220979974461,-1.,-1.76197817240128));
#23159=CARTESIAN_POINT('Ctrl Pts',(-0.75642189602781,-1.,-1.76789396002998));
#23160=CARTESIAN_POINT('Ctrl Pts',(-0.757578264077029,-1.,-1.77394167108292));
#23161=CARTESIAN_POINT('Ctrl Pts',(-0.758650626677518,-1.,-1.77999411220945));
#23162=CARTESIAN_POINT('Ctrl Pts',(-0.759614401110189,-1.,-1.78596964884604));
#23163=CARTESIAN_POINT('Ctrl Pts',(-0.760469555880749,-1.,-1.7918581561088));
#23164=CARTESIAN_POINT('Ctrl Pts',(-0.761229695230558,-1.,-1.79768986997783));
#23165=CARTESIAN_POINT('Ctrl Pts',(-0.761915336443547,-1.,-1.80351583877342));
#23166=CARTESIAN_POINT('Ctrl Pts',(-0.762546129463938,-1.,-1.80938551463965));
#23167=CARTESIAN_POINT('Ctrl Pts',(-0.763132003836634,-1.,-1.8153211840553));
#23168=CARTESIAN_POINT('Ctrl Pts',(-0.763673465462726,-1.,-1.82131873145266));
#23169=CARTESIAN_POINT('Ctrl Pts',(-0.764165902605995,-1.,-1.82735991200065));
#23170=CARTESIAN_POINT('Ctrl Pts',(-0.764602549687853,-1.,-1.83342077227142));
#23171=CARTESIAN_POINT('Ctrl Pts',(-0.764978057881737,-1.,-1.83948181064835));
#23172=CARTESIAN_POINT('Ctrl Pts',(-0.765291664862029,-1.,-1.84553698875924));
#23173=CARTESIAN_POINT('Ctrl Pts',(-0.765545710619062,-1.,-1.85158945130063));
#23174=CARTESIAN_POINT('Ctrl Pts',(-0.765744212909318,-1.,-1.85764741390394));
#23175=CARTESIAN_POINT('Ctrl Pts',(-0.765891519092547,-1.,-1.86372027063312));
#23176=CARTESIAN_POINT('Ctrl Pts',(-0.765990708546091,-1.,-1.86981398314341));
#23177=CARTESIAN_POINT('Ctrl Pts',(-0.766042837036744,-1.,-1.87592888967883));
#23178=CARTESIAN_POINT('Ctrl Pts',(-0.766047794851865,-1.,-1.88206215302561));
#23179=CARTESIAN_POINT('Ctrl Pts',(-0.766004837062091,-1.,-1.88820926433409));
#23180=CARTESIAN_POINT('Ctrl Pts',(-0.765913193856978,-1.,-1.89436577771388));
#23181=CARTESIAN_POINT('Ctrl Pts',(-0.765772772593386,-1.,-1.90052930393596));
#23182=CARTESIAN_POINT('Ctrl Pts',(-0.765584196937919,-1.,-1.90669961402356));
#23183=CARTESIAN_POINT('Ctrl Pts',(-0.765348465884722,-1.,-1.91287765805169));
#23184=CARTESIAN_POINT('Ctrl Pts',(-0.765066729667088,-1.,-1.91906491634196));
#23185=CARTESIAN_POINT('Ctrl Pts',(-0.764740025488211,-1.,-1.92526263537048));
#23186=CARTESIAN_POINT('Ctrl Pts',(-0.764369010673941,-1.,-1.93147105496382));
#23187=CARTESIAN_POINT('Ctrl Pts',(-0.763954049121458,-1.,-1.93768964875886));
#23188=CARTESIAN_POINT('Ctrl Pts',(-0.763495333538629,-1.,-1.9439174661764));
#23189=CARTESIAN_POINT('Ctrl Pts',(-0.762992990878769,-1.,-1.95015342590024));
#23190=CARTESIAN_POINT('Ctrl Pts',(-0.762447203806179,-1.,-1.95639665309869));
#23191=CARTESIAN_POINT('Ctrl Pts',(-0.761858300014423,-1.,-1.96264672744186));
#23192=CARTESIAN_POINT('Ctrl Pts',(-0.76122669048382,-1.,-1.96890351582499));
#23193=CARTESIAN_POINT('Ctrl Pts',(-0.760552825409757,-1.,-1.97516705321494));
#23194=CARTESIAN_POINT('Ctrl Pts',(-0.75983714745219,-1.,-1.98143741418172));
#23195=CARTESIAN_POINT('Ctrl Pts',(-0.759080037802488,-1.,-1.98771456680874));
#23196=CARTESIAN_POINT('Ctrl Pts',(-0.758281796766761,-1.,-1.99399831098817));
#23197=CARTESIAN_POINT('Ctrl Pts',(-0.757442676862724,-1.,-2.00028834739178));
#23198=CARTESIAN_POINT('Ctrl Pts',(-0.75656290464667,-1.,-2.0065843158773));
#23199=CARTESIAN_POINT('Ctrl Pts',(-0.755642704957865,-1.,-2.01288584328084));
#23200=CARTESIAN_POINT('Ctrl Pts',(-0.754682330722816,-1.,-2.01919259405809));
#23201=CARTESIAN_POINT('Ctrl Pts',(-0.753682061112768,-1.,-2.02550428623313));
#23202=CARTESIAN_POINT('Ctrl Pts',(-0.752642180487211,-1.,-2.03182068456221));
#23203=CARTESIAN_POINT('Ctrl Pts',(-0.751562963361115,-1.,-2.03814160092099));
#23204=CARTESIAN_POINT('Ctrl Pts',(-0.750444657875576,-1.,-2.04446689147979));
#23205=CARTESIAN_POINT('Ctrl Pts',(-0.749287468665046,-1.,-2.05079645592154));
#23206=CARTESIAN_POINT('Ctrl Pts',(-0.748091554183802,-1.,-2.05713023031006));
#23207=CARTESIAN_POINT('Ctrl Pts',(-0.747103932787919,-1.,-2.06220058927826));
#23208=CARTESIAN_POINT('Ctrl Pts',(-0.7463458715442,-1.,-2.06600523016815));
#23209=CARTESIAN_POINT('Ctrl Pts',(-0.745832791378367,-1.,-2.06854248895728));
#23210=CARTESIAN_POINT('Ctrl Pts',(-0.745574324794401,-1.,-2.0698113262342));
#23211=CARTESIAN_POINT('',(-0.61342227326009,-1.,-2.11275013067528));
#23212=CARTESIAN_POINT('',(-0.745574324794401,-1.,-2.0698113262342));
#23213=CARTESIAN_POINT('',(-0.383122945602004,-1.,-1.7075470150345));
#23214=CARTESIAN_POINT('Ctrl Pts',(-0.61342227326009,-1.,-2.11275013067528));
#23215=CARTESIAN_POINT('Ctrl Pts',(-0.6124673655618,-1.,-2.11187554259986));
#23216=CARTESIAN_POINT('Ctrl Pts',(-0.610560911689899,-1.,-2.11012443807238));
#23217=CARTESIAN_POINT('Ctrl Pts',(-0.607711315454876,-1.,-2.1074919961518));
#23218=CARTESIAN_POINT('Ctrl Pts',(-0.60393203073603,-1.,-2.10397049886949));
#23219=CARTESIAN_POINT('Ctrl Pts',(-0.599241616420533,-1.,-2.0995493086477));
#23220=CARTESIAN_POINT('Ctrl Pts',(-0.594585006052162,-1.,-2.0951087622027));
#23221=CARTESIAN_POINT('Ctrl Pts',(-0.589962365403406,-1.,-2.09064881812129));
#23222=CARTESIAN_POINT('Ctrl Pts',(-0.585373918991617,-1.,-2.08616943727951));
#23223=CARTESIAN_POINT('Ctrl Pts',(-0.580819952108063,-1.,-2.08167059018418));
#23224=CARTESIAN_POINT('Ctrl Pts',(-0.576300797416844,-1.,-2.07715226767559));
#23225=CARTESIAN_POINT('Ctrl Pts',(-0.571816823242603,-1.,-2.07261449292824));
#23226=CARTESIAN_POINT('Ctrl Pts',(-0.567368421181087,-1.,-2.06805732997334));
#23227=CARTESIAN_POINT('Ctrl Pts',(-0.562955993082261,-1.,-2.06348090160589));
#23228=CARTESIAN_POINT('Ctrl Pts',(-0.558579940185151,-1.,-2.05888537756462));
#23229=CARTESIAN_POINT('Ctrl Pts',(-0.554240657463906,-1.,-2.05427091604413));
#23230=CARTESIAN_POINT('Ctrl Pts',(-0.549938525150295,-1.,-2.04963761077958));
#23231=CARTESIAN_POINT('Ctrl Pts',(-0.54567390381743,-1.,-2.04498544714588));
#23232=CARTESIAN_POINT('Ctrl Pts',(-0.541447120615659,-1.,-2.04031422690527));
#23233=CARTESIAN_POINT('Ctrl Pts',(-0.537258489833262,-1.,-2.03562362954037));
#23234=CARTESIAN_POINT('Ctrl Pts',(-0.533108355132977,-1.,-2.03091336214426));
#23235=CARTESIAN_POINT('Ctrl Pts',(-0.528997127241914,-1.,-2.0261832908329));
#23236=CARTESIAN_POINT('Ctrl Pts',(-0.524925318333476,-1.,-2.02143356304698));
#23237=CARTESIAN_POINT('Ctrl Pts',(-0.52089359039937,-1.,-2.01666477917286));
#23238=CARTESIAN_POINT('Ctrl Pts',(-0.516902681728687,-1.,-2.01187773939242));
#23239=CARTESIAN_POINT('Ctrl Pts',(-0.512953306961792,-1.,-2.00707309946949));
#23240=CARTESIAN_POINT('Ctrl Pts',(-0.509046069886157,-1.,-2.00225107134734));
#23241=CARTESIAN_POINT('Ctrl Pts',(-0.505181361323026,-1.,-1.99741107463572));
#23242=CARTESIAN_POINT('Ctrl Pts',(-0.501359287727146,-1.,-1.99255149126155));
#23243=CARTESIAN_POINT('Ctrl Pts',(-0.497579909545574,-1.,-1.98767044752932));
#23244=CARTESIAN_POINT('Ctrl Pts',(-0.493843476541495,-1.,-1.98276658761821));
#23245=CARTESIAN_POINT('Ctrl Pts',(-0.490150627860952,-1.,-1.97783973019229));
#23246=CARTESIAN_POINT('Ctrl Pts',(-0.486502692907659,-1.,-1.97289186263272));
#23247=CARTESIAN_POINT('Ctrl Pts',(-0.482901662120691,-1.,-1.96792703422362));
#23248=CARTESIAN_POINT('Ctrl Pts',(-0.479349583074855,-1.,-1.96294933055943));
#23249=CARTESIAN_POINT('Ctrl Pts',(-0.475848034683176,-1.,-1.95796111148177));
#23250=CARTESIAN_POINT('Ctrl Pts',(-0.472397672264072,-1.,-1.95296148278133));
#23251=CARTESIAN_POINT('Ctrl Pts',(-0.468997482913135,-1.,-1.94794381136514));
#23252=CARTESIAN_POINT('Ctrl Pts',(-0.46564546202603,-1.,-1.9428979419619));
#23253=CARTESIAN_POINT('Ctrl Pts',(-0.462340031009056,-1.,-1.93781486640821));
#23254=CARTESIAN_POINT('Ctrl Pts',(-0.459081234547926,-1.,-1.93269066517934));
#23255=CARTESIAN_POINT('Ctrl Pts',(-0.455872005174371,-1.,-1.92753067150476));
#23256=CARTESIAN_POINT('Ctrl Pts',(-0.452719478359432,-1.,-1.92235380648502));
#23257=CARTESIAN_POINT('Ctrl Pts',(-0.449632260106662,-1.,-1.91718342555755));
#23258=CARTESIAN_POINT('Ctrl Pts',(-0.446617343485711,-1.,-1.9120369998112));
#23259=CARTESIAN_POINT('Ctrl Pts',(-0.443677556849151,-1.,-1.90691756144898));
#23260=CARTESIAN_POINT('Ctrl Pts',(-0.440807833704038,-1.,-1.90180124389086));
#23261=CARTESIAN_POINT('Ctrl Pts',(-0.437995003948244,-1.,-1.89663648956466));
#23262=CARTESIAN_POINT('Ctrl Pts',(-0.435225660963383,-1.,-1.89136993975504));
#23263=CARTESIAN_POINT('Ctrl Pts',(-0.432493038548748,-1.,-1.88596913666793));
#23264=CARTESIAN_POINT('Ctrl Pts',(-0.429803062482344,-1.,-1.88044229001832));
#23265=CARTESIAN_POINT('Ctrl Pts',(-0.427183828519102,-1.,-1.87486989291484));
#23266=CARTESIAN_POINT('Ctrl Pts',(-0.424678177291359,-1.,-1.86937803944323));
#23267=CARTESIAN_POINT('Ctrl Pts',(-0.422327307418275,-1.,-1.86408083334028));
#23268=CARTESIAN_POINT('Ctrl Pts',(-0.420157287975619,-1.,-1.85903281096686));
#23269=CARTESIAN_POINT('Ctrl Pts',(-0.418164129143534,-1.,-1.85417632856234));
#23270=CARTESIAN_POINT('Ctrl Pts',(-0.416300022038864,-1.,-1.84929312929882));
#23271=CARTESIAN_POINT('Ctrl Pts',(-0.41448743825434,-1.,-1.8440575707371));
#23272=CARTESIAN_POINT('Ctrl Pts',(-0.412633125322162,-1.,-1.83808953475839));
#23273=CARTESIAN_POINT('Ctrl Pts',(-0.410641256301675,-1.,-1.83100408895216));
#23274=CARTESIAN_POINT('Ctrl Pts',(-0.408428948108533,-1.,-1.8224702267854));
#23275=CARTESIAN_POINT('Ctrl Pts',(-0.405933518411838,-1.,-1.81223801813988));
#23276=CARTESIAN_POINT('Ctrl Pts',(-0.403107976170441,-1.,-1.80012077176221));
#23277=CARTESIAN_POINT('Ctrl Pts',(-0.39991940378308,-1.,-1.78598826347533));
#23278=CARTESIAN_POINT('Ctrl Pts',(-0.39634619612042,-1.,-1.7697556004756));
#23279=CARTESIAN_POINT('Ctrl Pts',(-0.392375812294307,-1.,-1.75137405313962));
#23280=CARTESIAN_POINT('Ctrl Pts',(-0.388877023509191,-1.,-1.7349317097561));
#23281=CARTESIAN_POINT('Ctrl Pts',(-0.38607079032701,-1.,-1.72162022246158));
#23282=CARTESIAN_POINT('Ctrl Pts',(-0.384119047315542,-1.,-1.71231062891958));
#23283=CARTESIAN_POINT('Ctrl Pts',(-0.383122945602004,-1.,-1.7075470150345));
#23284=CARTESIAN_POINT('',(-0.163289472382896,-1.,-1.74236521665491));
#23285=CARTESIAN_POINT('Origin',(0.,-1.,0.));
#23286=CARTESIAN_POINT('',(-0.0694764450219581,-1.,-2.19890268624765));
#23287=CARTESIAN_POINT('Ctrl Pts',(-0.163289472382896,-1.,-1.74236521665491));
#23288=CARTESIAN_POINT('Ctrl Pts',(-0.163814161002002,-1.,-1.7472034950333));
#23289=CARTESIAN_POINT('Ctrl Pts',(-0.164834765707158,-1.,-1.75666056638427));
#23290=CARTESIAN_POINT('Ctrl Pts',(-0.1662793551464,-1.,-1.77018771684844));
#23291=CARTESIAN_POINT('Ctrl Pts',(-0.168032772805197,-1.,-1.7869064998507));
#23292=CARTESIAN_POINT('Ctrl Pts',(-0.169936923904608,-1.,-1.80561530629706));
#23293=CARTESIAN_POINT('Ctrl Pts',(-0.171554770204119,-1.,-1.82215766811545));
#23294=CARTESIAN_POINT('Ctrl Pts',(-0.1728894428919,-1.,-1.83658380527692));
#23295=CARTESIAN_POINT('Ctrl Pts',(-0.173946627587731,-1.,-1.8489811319852));
#23296=CARTESIAN_POINT('Ctrl Pts',(-0.17473525927603,-1.,-1.85948367088837));
#23297=CARTESIAN_POINT('Ctrl Pts',(-0.175268337590758,-1.,-1.86828349694799));
#23298=CARTESIAN_POINT('Ctrl Pts',(-0.175563480746485,-1.,-1.87563767773588));
#23299=CARTESIAN_POINT('Ctrl Pts',(-0.175644148889699,-1.,-1.88188663145367));
#23300=CARTESIAN_POINT('Ctrl Pts',(-0.175538155840648,-1.,-1.88742606273259));
#23301=CARTESIAN_POINT('Ctrl Pts',(-0.175274276190844,-1.,-1.892646301985));
#23302=CARTESIAN_POINT('Ctrl Pts',(-0.174879405091263,-1.,-1.89788101117132));
#23303=CARTESIAN_POINT('Ctrl Pts',(-0.174375518661085,-1.,-1.90335253862834));
#23304=CARTESIAN_POINT('Ctrl Pts',(-0.173776635257817,-1.,-1.90911693975267));
#23305=CARTESIAN_POINT('Ctrl Pts',(-0.173090695383496,-1.,-1.91511429159527));
#23306=CARTESIAN_POINT('Ctrl Pts',(-0.172321621259514,-1.,-1.9212233439798));
#23307=CARTESIAN_POINT('Ctrl Pts',(-0.171471191532988,-1.,-1.92731093582036));
#23308=CARTESIAN_POINT('Ctrl Pts',(-0.170541253116202,-1.,-1.93329183155539));
#23309=CARTESIAN_POINT('Ctrl Pts',(-0.169534904817491,-1.,-1.93915639211581));
#23310=CARTESIAN_POINT('Ctrl Pts',(-0.168455741607556,-1.,-1.94493757756931));
#23311=CARTESIAN_POINT('Ctrl Pts',(-0.167307501784475,-1.,-1.95069027794294));
#23312=CARTESIAN_POINT('Ctrl Pts',(-0.166093592002812,-1.,-1.9564675971873));
#23313=CARTESIAN_POINT('Ctrl Pts',(-0.164816568920269,-1.,-1.96229379940136));
#23314=CARTESIAN_POINT('Ctrl Pts',(-0.163478185457734,-1.,-1.96816512677967));
#23315=CARTESIAN_POINT('Ctrl Pts',(-0.162079693556289,-1.,-1.97406280235188));
#23316=CARTESIAN_POINT('Ctrl Pts',(-0.160622060784611,-1.,-1.97996195437559));
#23317=CARTESIAN_POINT('Ctrl Pts',(-0.159106226437299,-1.,-1.98584238283292));
#23318=CARTESIAN_POINT('Ctrl Pts',(-0.157533331459227,-1.,-1.99169810931908));
#23319=CARTESIAN_POINT('Ctrl Pts',(-0.155904629548783,-1.,-1.99753284771497));
#23320=CARTESIAN_POINT('Ctrl Pts',(-0.154221403049722,-1.,-2.00335565310543));
#23321=CARTESIAN_POINT('Ctrl Pts',(-0.15248488362145,-1.,-2.00917680318424));
#23322=CARTESIAN_POINT('Ctrl Pts',(-0.150696157673078,-1.,-2.01500291940238));
#23323=CARTESIAN_POINT('Ctrl Pts',(-0.148856124775337,-1.,-2.02083464969894));
#23324=CARTESIAN_POINT('Ctrl Pts',(-0.146965557332583,-1.,-2.02666926182017));
#23325=CARTESIAN_POINT('Ctrl Pts',(-0.145025140186057,-1.,-2.03250223739942));
#23326=CARTESIAN_POINT('Ctrl Pts',(-0.143035515058209,-1.,-2.03832911025912));
#23327=CARTESIAN_POINT('Ctrl Pts',(-0.140997332152546,-1.,-2.04414757947916));
#23328=CARTESIAN_POINT('Ctrl Pts',(-0.138911255368966,-1.,-2.04995762001328));
#23329=CARTESIAN_POINT('Ctrl Pts',(-0.136777941218044,-1.,-2.05576044414264));
#23330=CARTESIAN_POINT('Ctrl Pts',(-0.134598026192106,-1.,-2.06155781517842));
#23331=CARTESIAN_POINT('Ctrl Pts',(-0.13237211154771,-1.,-2.06735123910326));
#23332=CARTESIAN_POINT('Ctrl Pts',(-0.130100748328403,-1.,-2.07314114713063));
#23333=CARTESIAN_POINT('Ctrl Pts',(-0.12778444527612,-1.,-2.07892715110987));
#23334=CARTESIAN_POINT('Ctrl Pts',(-0.125423679412061,-1.,-2.08470840653643));
#23335=CARTESIAN_POINT('Ctrl Pts',(-0.123018905621083,-1.,-2.09048392424825));
#23336=CARTESIAN_POINT('Ctrl Pts',(-0.120570567965122,-1.,-2.0962529286773));
#23337=CARTESIAN_POINT('Ctrl Pts',(-0.118079107988355,-1.,-2.102015121329));
#23338=CARTESIAN_POINT('Ctrl Pts',(-0.115544957687926,-1.,-2.10777050261309));
#23339=CARTESIAN_POINT('Ctrl Pts',(-0.112968534419737,-1.,-2.11351924490306));
#23340=CARTESIAN_POINT('Ctrl Pts',(-0.110350236135025,-1.,-2.11926155590865));
#23341=CARTESIAN_POINT('Ctrl Pts',(-0.10769043523109,-1.,-2.12499752307));
#23342=CARTESIAN_POINT('Ctrl Pts',(-0.104989479152739,-1.,-2.13072704887293));
#23343=CARTESIAN_POINT('Ctrl Pts',(-0.1022477005561,-1.,-2.13644992667165));
#23344=CARTESIAN_POINT('Ctrl Pts',(-0.0994654261990915,-1.,-2.14216588396025));
#23345=CARTESIAN_POINT('Ctrl Pts',(-0.0966429852305459,-1.,-2.14787463531795));
#23346=CARTESIAN_POINT('Ctrl Pts',(-0.0937807218867643,-1.,-2.1535759397817));
#23347=CARTESIAN_POINT('Ctrl Pts',(-0.0908789888107265,-1.,-2.15926961544516));
#23348=CARTESIAN_POINT('Ctrl Pts',(-0.0879381291386923,-1.,-2.16495552645014));
#23349=CARTESIAN_POINT('Ctrl Pts',(-0.0849584620835372,-1.,-2.17063357870952));
#23350=CARTESIAN_POINT('Ctrl Pts',(-0.0819402680872765,-1.,-2.176303712113));
#23351=CARTESIAN_POINT('Ctrl Pts',(-0.0788837727685243,-1.,-2.18196589448887));
#23352=CARTESIAN_POINT('Ctrl Pts',(-0.0757891465836148,-1.,-2.1876201139953));
#23353=CARTESIAN_POINT('Ctrl Pts',(-0.0732830357306725,-1.,-2.19213712013662));
#23354=CARTESIAN_POINT('Ctrl Pts',(-0.0713863779526154,-1.,-2.19552129484002));
#23355=CARTESIAN_POINT('Ctrl Pts',(-0.070114353632549,-1.,-2.19777582085423));
#23356=CARTESIAN_POINT('Ctrl Pts',(-0.0694764450219581,-1.,-2.19890268624765));
#23357=CARTESIAN_POINT('',(0.0694764450219584,-1.,-2.19890268624765));
#23358=CARTESIAN_POINT('',(-0.0694764450219581,-1.,-2.19890268624765));
#23359=CARTESIAN_POINT('',(0.163289472382896,-1.,-1.74236521665491));
#23360=CARTESIAN_POINT('Ctrl Pts',(0.0694764450219584,-1.,-2.19890268624765));
#23361=CARTESIAN_POINT('Ctrl Pts',(0.0701143536324926,-1.,-2.19777582085261));
#23362=CARTESIAN_POINT('Ctrl Pts',(0.0713863779524627,-1.,-2.19552129483562));
#23363=CARTESIAN_POINT('Ctrl Pts',(0.0732830357304276,-1.,-2.19213712012956));
#23364=CARTESIAN_POINT('Ctrl Pts',(0.0757891465833411,-1.,-2.1876201139874));
#23365=CARTESIAN_POINT('Ctrl Pts',(0.0788837727683228,-1.,-2.18196589448304));
#23366=CARTESIAN_POINT('Ctrl Pts',(0.0819402680871939,-1.,-2.1763037121106));
#23367=CARTESIAN_POINT('Ctrl Pts',(0.0849584620835643,-1.,-2.17063357871031));
#23368=CARTESIAN_POINT('Ctrl Pts',(0.0879381291387823,-1.,-2.16495552645275));
#23369=CARTESIAN_POINT('Ctrl Pts',(0.0908789888108266,-1.,-2.15926961544808));
#23370=CARTESIAN_POINT('Ctrl Pts',(0.0937807218868345,-1.,-2.15357593978377));
#23371=CARTESIAN_POINT('Ctrl Pts',(0.0966429852305689,-1.,-2.14787463531864));
#23372=CARTESIAN_POINT('Ctrl Pts',(0.0994654261990743,-1.,-2.14216588395974));
#23373=CARTESIAN_POINT('Ctrl Pts',(0.102247700556064,-1.,-2.13644992667052));
#23374=CARTESIAN_POINT('Ctrl Pts',(0.104989479152703,-1.,-2.1307270488718));
#23375=CARTESIAN_POINT('Ctrl Pts',(0.107690435231068,-1.,-2.12499752306927));
#23376=CARTESIAN_POINT('Ctrl Pts',(0.11035023613502,-1.,-2.11926155590849));
#23377=CARTESIAN_POINT('Ctrl Pts',(0.112968534419746,-1.,-2.11351924490335));
#23378=CARTESIAN_POINT('Ctrl Pts',(0.11554495768794,-1.,-2.10777050261359));
#23379=CARTESIAN_POINT('Ctrl Pts',(0.118079107988368,-1.,-2.10201512132945));
#23380=CARTESIAN_POINT('Ctrl Pts',(0.120570567965129,-1.,-2.09625292867756));
#23381=CARTESIAN_POINT('Ctrl Pts',(0.123018905621083,-1.,-2.09048392424826));
#23382=CARTESIAN_POINT('Ctrl Pts',(0.125423679412058,-1.,-2.08470840653628));
#23383=CARTESIAN_POINT('Ctrl Pts',(0.127784445276116,-1.,-2.07892715110967));
#23384=CARTESIAN_POINT('Ctrl Pts',(0.1301007483284,-1.,-2.07314114713047));
#23385=CARTESIAN_POINT('Ctrl Pts',(0.13237211154771,-1.,-2.06735123910319));
#23386=CARTESIAN_POINT('Ctrl Pts',(0.134598026192107,-1.,-2.06155781517844));
#23387=CARTESIAN_POINT('Ctrl Pts',(0.136777941218044,-1.,-2.0557604441427));
#23388=CARTESIAN_POINT('Ctrl Pts',(0.138911255368966,-1.,-2.04995762001333));
#23389=CARTESIAN_POINT('Ctrl Pts',(0.140997332152545,-1.,-2.04414757947919));
#23390=CARTESIAN_POINT('Ctrl Pts',(0.143035515058208,-1.,-2.03832911025913));
#23391=CARTESIAN_POINT('Ctrl Pts',(0.145025140186058,-1.,-2.03250223739941));
#23392=CARTESIAN_POINT('Ctrl Pts',(0.146965557332586,-1.,-2.02666926182017));
#23393=CARTESIAN_POINT('Ctrl Pts',(0.148856124775343,-1.,-2.02083464969897));
#23394=CARTESIAN_POINT('Ctrl Pts',(0.150696157673084,-1.,-2.01500291940243));
#23395=CARTESIAN_POINT('Ctrl Pts',(0.152484883621452,-1.,-2.00917680318426));
#23396=CARTESIAN_POINT('Ctrl Pts',(0.154221403049719,-1.,-2.00335565310539));
#23397=CARTESIAN_POINT('Ctrl Pts',(0.155904629548774,-1.,-1.99753284771487));
#23398=CARTESIAN_POINT('Ctrl Pts',(0.157533331459215,-1.,-1.99169810931893));
#23399=CARTESIAN_POINT('Ctrl Pts',(0.159106226437288,-1.,-1.98584238283279));
#23400=CARTESIAN_POINT('Ctrl Pts',(0.16062206078461,-1.,-1.97996195437557));
#23401=CARTESIAN_POINT('Ctrl Pts',(0.162079693556302,-1.,-1.97406280235204));
#23402=CARTESIAN_POINT('Ctrl Pts',(0.16347818545776,-1.,-1.96816512678));
#23403=CARTESIAN_POINT('Ctrl Pts',(0.1648165689203,-1.,-1.96229379940174));
#23404=CARTESIAN_POINT('Ctrl Pts',(0.166093592002833,-1.,-1.95646759718755));
#23405=CARTESIAN_POINT('Ctrl Pts',(0.167307501784469,-1.,-1.95069027794286));
#23406=CARTESIAN_POINT('Ctrl Pts',(0.168455741607516,-1.,-1.94493757756879));
#23407=CARTESIAN_POINT('Ctrl Pts',(0.169534904817425,-1.,-1.93915639211497));
#23408=CARTESIAN_POINT('Ctrl Pts',(0.170541253116136,-1.,-1.93329183155455));
#23409=CARTESIAN_POINT('Ctrl Pts',(0.17147119153296,-1.,-1.92731093582));
#23410=CARTESIAN_POINT('Ctrl Pts',(0.172321621259557,-1.,-1.92122334398034));
#23411=CARTESIAN_POINT('Ctrl Pts',(0.173090695383619,-1.,-1.91511429159681));
#23412=CARTESIAN_POINT('Ctrl Pts',(0.173776635257984,-1.,-1.90911693975475));
#23413=CARTESIAN_POINT('Ctrl Pts',(0.174375518661222,-1.,-1.90335253863003));
#23414=CARTESIAN_POINT('Ctrl Pts',(0.174879405091277,-1.,-1.89788101117148));
#23415=CARTESIAN_POINT('Ctrl Pts',(0.175274276190664,-1.,-1.89264630198279));
#23416=CARTESIAN_POINT('Ctrl Pts',(0.175538155840286,-1.,-1.88742606272818));
#23417=CARTESIAN_POINT('Ctrl Pts',(0.175644148889271,-1.,-1.88188663144846));
#23418=CARTESIAN_POINT('Ctrl Pts',(0.175563480746205,-1.,-1.87563767773249));
#23419=CARTESIAN_POINT('Ctrl Pts',(0.175268337590901,-1.,-1.86828349694972));
#23420=CARTESIAN_POINT('Ctrl Pts',(0.174735259276856,-1.,-1.85948367089838));
#23421=CARTESIAN_POINT('Ctrl Pts',(0.173946627589401,-1.,-1.84898113200543));
#23422=CARTESIAN_POINT('Ctrl Pts',(0.17288944289442,-1.,-1.83658380530747));
#23423=CARTESIAN_POINT('Ctrl Pts',(0.171554770207306,-1.,-1.82215766815414));
#23424=CARTESIAN_POINT('Ctrl Pts',(0.169936923908078,-1.,-1.80561530633924));
#23425=CARTESIAN_POINT('Ctrl Pts',(0.16803277280837,-1.,-1.78690649988931));
#23426=CARTESIAN_POINT('Ctrl Pts',(0.166279355148738,-1.,-1.77018771687692));
#23427=CARTESIAN_POINT('Ctrl Pts',(0.164834765708484,-1.,-1.75666056640041));
#23428=CARTESIAN_POINT('Ctrl Pts',(0.163814161002474,-1.,-1.74720349503904));
#23429=CARTESIAN_POINT('Ctrl Pts',(0.163289472382896,-1.,-1.74236521665491));
#23430=CARTESIAN_POINT('',(0.383122945602004,-1.,-1.7075470150345));
#23431=CARTESIAN_POINT('Origin',(0.,-1.,0.));
#23432=CARTESIAN_POINT('',(0.61342227326009,-1.,-2.11275013067528));
#23433=CARTESIAN_POINT('Ctrl Pts',(0.383122945602004,-1.,-1.7075470150345));
#23434=CARTESIAN_POINT('Ctrl Pts',(0.384119047314215,-1.,-1.71231062891398));
#23435=CARTESIAN_POINT('Ctrl Pts',(0.386070790323281,-1.,-1.72162022244582));
#23436=CARTESIAN_POINT('Ctrl Pts',(0.388877023502615,-1.,-1.73493170972829));
#23437=CARTESIAN_POINT('Ctrl Pts',(0.392375812285395,-1.,-1.75137405310193));
#23438=CARTESIAN_POINT('Ctrl Pts',(0.396346196110688,-1.,-1.76975560043442));
#23439=CARTESIAN_POINT('Ctrl Pts',(0.399919403774155,-1.,-1.78598826343754));
#23440=CARTESIAN_POINT('Ctrl Pts',(0.403107976163396,-1.,-1.80012077173238));
#23441=CARTESIAN_POINT('Ctrl Pts',(0.405933518407175,-1.,-1.81223801812013));
#23442=CARTESIAN_POINT('Ctrl Pts',(0.408428948106227,-1.,-1.82247022677562));
#23443=CARTESIAN_POINT('Ctrl Pts',(0.410641256301276,-1.,-1.83100408895047));
#23444=CARTESIAN_POINT('Ctrl Pts',(0.412633125322945,-1.,-1.8380895347617));
#23445=CARTESIAN_POINT('Ctrl Pts',(0.414487438255542,-1.,-1.84405757074218));
#23446=CARTESIAN_POINT('Ctrl Pts',(0.416300022039885,-1.,-1.84929312930314));
#23447=CARTESIAN_POINT('Ctrl Pts',(0.418164129144045,-1.,-1.8541763285645));
#23448=CARTESIAN_POINT('Ctrl Pts',(0.420157287975583,-1.,-1.8590328109667));
#23449=CARTESIAN_POINT('Ctrl Pts',(0.422327307417884,-1.,-1.86408083333863));
#23450=CARTESIAN_POINT('Ctrl Pts',(0.424678177290876,-1.,-1.8693780394412));
#23451=CARTESIAN_POINT('Ctrl Pts',(0.427183828518743,-1.,-1.87486989291334));
#23452=CARTESIAN_POINT('Ctrl Pts',(0.429803062482217,-1.,-1.88044229001779));
#23453=CARTESIAN_POINT('Ctrl Pts',(0.432493038548833,-1.,-1.88596913666828));
#23454=CARTESIAN_POINT('Ctrl Pts',(0.43522566096358,-1.,-1.89136993975585));
#23455=CARTESIAN_POINT('Ctrl Pts',(0.437995003948443,-1.,-1.89663648956549));
#23456=CARTESIAN_POINT('Ctrl Pts',(0.44080783370416,-1.,-1.90180124389137));
#23457=CARTESIAN_POINT('Ctrl Pts',(0.44367755684917,-1.,-1.90691756144906));
#23458=CARTESIAN_POINT('Ctrl Pts',(0.446617343485651,-1.,-1.91203699981095));
#23459=CARTESIAN_POINT('Ctrl Pts',(0.449632260106572,-1.,-1.91718342555717));
#23460=CARTESIAN_POINT('Ctrl Pts',(0.452719478359356,-1.,-1.9223538064847));
#23461=CARTESIAN_POINT('Ctrl Pts',(0.455872005174335,-1.,-1.92753067150461));
#23462=CARTESIAN_POINT('Ctrl Pts',(0.459081234547931,-1.,-1.93269066517936));
#23463=CARTESIAN_POINT('Ctrl Pts',(0.462340031009087,-1.,-1.93781486640834));
#23464=CARTESIAN_POINT('Ctrl Pts',(0.465645462026064,-1.,-1.94289794196205));
#23465=CARTESIAN_POINT('Ctrl Pts',(0.468997482913158,-1.,-1.94794381136524));
#23466=CARTESIAN_POINT('Ctrl Pts',(0.472397672264079,-1.,-1.95296148278136));
#23467=CARTESIAN_POINT('Ctrl Pts',(0.475848034683171,-1.,-1.95796111148175));
#23468=CARTESIAN_POINT('Ctrl Pts',(0.479349583074846,-1.,-1.96294933055938));
#23469=CARTESIAN_POINT('Ctrl Pts',(0.482901662120686,-1.,-1.96792703422358));
#23470=CARTESIAN_POINT('Ctrl Pts',(0.486502692907661,-1.,-1.97289186263272));
#23471=CARTESIAN_POINT('Ctrl Pts',(0.490150627860955,-1.,-1.97783973019229));
#23472=CARTESIAN_POINT('Ctrl Pts',(0.493843476541492,-1.,-1.9827665876182));
#23473=CARTESIAN_POINT('Ctrl Pts',(0.497579909545564,-1.,-1.98767044752929));
#23474=CARTESIAN_POINT('Ctrl Pts',(0.501359287727129,-1.,-1.9925514912615));
#23475=CARTESIAN_POINT('Ctrl Pts',(0.505181361323011,-1.,-1.99741107463567));
#23476=CARTESIAN_POINT('Ctrl Pts',(0.509046069886152,-1.,-2.00225107134733));
#23477=CARTESIAN_POINT('Ctrl Pts',(0.512953306961813,-1.,-2.00707309946955));
#23478=CARTESIAN_POINT('Ctrl Pts',(0.516902681728733,-1.,-2.01187773939257));
#23479=CARTESIAN_POINT('Ctrl Pts',(0.520893590399428,-1.,-2.01666477917306));
#23480=CARTESIAN_POINT('Ctrl Pts',(0.524925318333518,-1.,-2.02143356304712));
#23481=CARTESIAN_POINT('Ctrl Pts',(0.52899712724191,-1.,-2.02618329083289));
#23482=CARTESIAN_POINT('Ctrl Pts',(0.533108355132905,-1.,-2.03091336214401));
#23483=CARTESIAN_POINT('Ctrl Pts',(0.537258489833134,-1.,-2.03562362953993));
#23484=CARTESIAN_POINT('Ctrl Pts',(0.54144712061552,-1.,-2.0403142269048));
#23485=CARTESIAN_POINT('Ctrl Pts',(0.545673903817348,-1.,-2.0449854471456));
#23486=CARTESIAN_POINT('Ctrl Pts',(0.549938525150342,-1.,-2.04963761077974));
#23487=CARTESIAN_POINT('Ctrl Pts',(0.554240657464109,-1.,-2.05427091604482));
#23488=CARTESIAN_POINT('Ctrl Pts',(0.558579940185467,-1.,-2.05888537756571));
#23489=CARTESIAN_POINT('Ctrl Pts',(0.562955993082574,-1.,-2.06348090160697));
#23490=CARTESIAN_POINT('Ctrl Pts',(0.567368421181229,-1.,-2.06805732997383));
#23491=CARTESIAN_POINT('Ctrl Pts',(0.571816823242411,-1.,-2.07261449292758));
#23492=CARTESIAN_POINT('Ctrl Pts',(0.576300797416274,-1.,-2.07715226767361));
#23493=CARTESIAN_POINT('Ctrl Pts',(0.580819952107256,-1.,-2.08167059018138));
#23494=CARTESIAN_POINT('Ctrl Pts',(0.585373918990895,-1.,-2.086169437277));
#23495=CARTESIAN_POINT('Ctrl Pts',(0.589962365403189,-1.,-2.09064881812053));
#23496=CARTESIAN_POINT('Ctrl Pts',(0.594585006052823,-1.,-2.09510876220501));
#23497=CARTESIAN_POINT('Ctrl Pts',(0.599241616422144,-1.,-2.09954930865331));
#23498=CARTESIAN_POINT('Ctrl Pts',(0.603932030738212,-1.,-2.10397049887709));
#23499=CARTESIAN_POINT('Ctrl Pts',(0.607711315456826,-1.,-2.10749199615859));
#23500=CARTESIAN_POINT('Ctrl Pts',(0.610560911691113,-1.,-2.11012443807661));
#23501=CARTESIAN_POINT('Ctrl Pts',(0.61246736556225,-1.,-2.11187554260142));
#23502=CARTESIAN_POINT('Ctrl Pts',(0.61342227326009,-1.,-2.11275013067528));
#23503=CARTESIAN_POINT('',(0.745574324794401,-1.,-2.0698113262342));
#23504=CARTESIAN_POINT('',(0.61342227326009,-1.,-2.11275013067528));
#23505=CARTESIAN_POINT('',(0.693717979106306,-1.,-1.60662857109684));
#23506=CARTESIAN_POINT('Ctrl Pts',(0.745574324794401,-1.,-2.0698113262342));
#23507=CARTESIAN_POINT('Ctrl Pts',(0.74583279137781,-1.,-2.06854248895575));
#23508=CARTESIAN_POINT('Ctrl Pts',(0.746345871542695,-1.,-2.06600523016401));
#23509=CARTESIAN_POINT('Ctrl Pts',(0.747103932785504,-1.,-2.06220058927162));
#23510=CARTESIAN_POINT('Ctrl Pts',(0.748091554181101,-1.,-2.05713023030263));
#23511=CARTESIAN_POINT('Ctrl Pts',(0.749287468663053,-1.,-2.05079645591606));
#23512=CARTESIAN_POINT('Ctrl Pts',(0.750444657874758,-1.,-2.04446689147754));
#23513=CARTESIAN_POINT('Ctrl Pts',(0.751562963361383,-1.,-2.03814160092173));
#23514=CARTESIAN_POINT('Ctrl Pts',(0.752642180488104,-1.,-2.03182068456467));
#23515=CARTESIAN_POINT('Ctrl Pts',(0.753682061113765,-1.,-2.02550428623587));
#23516=CARTESIAN_POINT('Ctrl Pts',(0.75468233072352,-1.,-2.01919259406003));
#23517=CARTESIAN_POINT('Ctrl Pts',(0.7556427049581,-1.,-2.01288584328149));
#23518=CARTESIAN_POINT('Ctrl Pts',(0.756562904646496,-1.,-2.00658431587682));
#23519=CARTESIAN_POINT('Ctrl Pts',(0.757442676862341,-1.,-2.00028834739072));
#23520=CARTESIAN_POINT('Ctrl Pts',(0.758281796766377,-1.,-1.9939983109871));
#23521=CARTESIAN_POINT('Ctrl Pts',(0.759080037802242,-1.,-1.98771456680806));
#23522=CARTESIAN_POINT('Ctrl Pts',(0.759837147452135,-1.,-1.98143741418156));
#23523=CARTESIAN_POINT('Ctrl Pts',(0.760552825409855,-1.,-1.97516705321521));
#23524=CARTESIAN_POINT('Ctrl Pts',(0.761226690483986,-1.,-1.96890351582545));
#23525=CARTESIAN_POINT('Ctrl Pts',(0.761858300014575,-1.,-1.96264672744229));
#23526=CARTESIAN_POINT('Ctrl Pts',(0.762447203806263,-1.,-1.95639665309893));
#23527=CARTESIAN_POINT('Ctrl Pts',(0.762992990878774,-1.,-1.95015342590025));
#23528=CARTESIAN_POINT('Ctrl Pts',(0.76349533353858,-1.,-1.94391746617626));
#23529=CARTESIAN_POINT('Ctrl Pts',(0.763954049121393,-1.,-1.93768964875867));
#23530=CARTESIAN_POINT('Ctrl Pts',(0.764369010673889,-1.,-1.93147105496367));
#23531=CARTESIAN_POINT('Ctrl Pts',(0.764740025488189,-1.,-1.92526263537041));
#23532=CARTESIAN_POINT('Ctrl Pts',(0.765066729667095,-1.,-1.91906491634197));
#23533=CARTESIAN_POINT('Ctrl Pts',(0.765348465884739,-1.,-1.91287765805174));
#23534=CARTESIAN_POINT('Ctrl Pts',(0.765584196937936,-1.,-1.90669961402362));
#23535=CARTESIAN_POINT('Ctrl Pts',(0.765772772593395,-1.,-1.90052930393599));
#23536=CARTESIAN_POINT('Ctrl Pts',(0.765913193856979,-1.,-1.89436577771389));
#23537=CARTESIAN_POINT('Ctrl Pts',(0.76600483706209,-1.,-1.88820926433409));
#23538=CARTESIAN_POINT('Ctrl Pts',(0.766047794851868,-1.,-1.88206215302561));
#23539=CARTESIAN_POINT('Ctrl Pts',(0.766042837036759,-1.,-1.87592888967886));
#23540=CARTESIAN_POINT('Ctrl Pts',(0.765990708546111,-1.,-1.86981398314345));
#23541=CARTESIAN_POINT('Ctrl Pts',(0.765891519092557,-1.,-1.86372027063315));
#23542=CARTESIAN_POINT('Ctrl Pts',(0.765744212909305,-1.,-1.85764741390391));
#23543=CARTESIAN_POINT('Ctrl Pts',(0.765545710619023,-1.,-1.85158945130054));
#23544=CARTESIAN_POINT('Ctrl Pts',(0.765291664861971,-1.,-1.84553698875911));
#23545=CARTESIAN_POINT('Ctrl Pts',(0.764978057881687,-1.,-1.83948181064823));
#23546=CARTESIAN_POINT('Ctrl Pts',(0.764602549687845,-1.,-1.8334207722714));
#23547=CARTESIAN_POINT('Ctrl Pts',(0.764165902606055,-1.,-1.8273599120008));
#23548=CARTESIAN_POINT('Ctrl Pts',(0.763673465462854,-1.,-1.82131873145297));
#23549=CARTESIAN_POINT('Ctrl Pts',(0.763132003836783,-1.,-1.81532118405566));
#23550=CARTESIAN_POINT('Ctrl Pts',(0.762546129464036,-1.,-1.80938551463989));
#23551=CARTESIAN_POINT('Ctrl Pts',(0.761915336443515,-1.,-1.80351583877334));
#23552=CARTESIAN_POINT('Ctrl Pts',(0.761229695230359,-1.,-1.79768986997735));
#23553=CARTESIAN_POINT('Ctrl Pts',(0.760469555880425,-1.,-1.79185815610802));
#23554=CARTESIAN_POINT('Ctrl Pts',(0.759614401109868,-1.,-1.78596964884527));
#23555=CARTESIAN_POINT('Ctrl Pts',(0.75865062667738,-1.,-1.77999411220912));
#23556=CARTESIAN_POINT('Ctrl Pts',(0.757578264077238,-1.,-1.77394167108342));
#23557=CARTESIAN_POINT('Ctrl Pts',(0.756421896028403,-1.,-1.76789396003141));
#23558=CARTESIAN_POINT('Ctrl Pts',(0.755220979975262,-1.,-1.7619781724032));
#23559=CARTESIAN_POINT('Ctrl Pts',(0.75400925402848,-1.,-1.75631083600175));
#23560=CARTESIAN_POINT('Ctrl Pts',(0.752797683531377,-1.,-1.75095139468809));
#23561=CARTESIAN_POINT('Ctrl Pts',(0.751555614163629,-1.,-1.74585086852298));
#23562=CARTESIAN_POINT('Ctrl Pts',(0.75019343597954,-1.,-1.74080458266705));
#23563=CARTESIAN_POINT('Ctrl Pts',(0.748582462954854,-1.,-1.73550351679848));
#23564=CARTESIAN_POINT('Ctrl Pts',(0.746574710096436,-1.,-1.72958533647399));
#23565=CARTESIAN_POINT('Ctrl Pts',(0.744021445433764,-1.,-1.7226822991693));
#23566=CARTESIAN_POINT('Ctrl Pts',(0.740795162032087,-1.,-1.71447789751927));
#23567=CARTESIAN_POINT('Ctrl Pts',(0.736799665724771,-1.,-1.70473309006121));
#23568=CARTESIAN_POINT('Ctrl Pts',(0.731963238697195,-1.,-1.69326921975743));
#23569=CARTESIAN_POINT('Ctrl Pts',(0.726235967997433,-1.,-1.67996158455503));
#23570=CARTESIAN_POINT('Ctrl Pts',(0.719585433804282,-1.,-1.6647288055568));
#23571=CARTESIAN_POINT('Ctrl Pts',(0.711993139355394,-1.,-1.64752408832016));
#23572=CARTESIAN_POINT('Ctrl Pts',(0.705159151988319,-1.,-1.63216541664676));
#23573=CARTESIAN_POINT('Ctrl Pts',(0.699605146405088,-1.,-1.61974673472612));
#23574=CARTESIAN_POINT('Ctrl Pts',(0.695712097881194,-1.,-1.61106790958151));
#23575=CARTESIAN_POINT('Ctrl Pts',(0.693717979106306,-1.,-1.60662857109684));
#23576=CARTESIAN_POINT('',(0.892032620296855,-1.,-1.5055822144029));
#23577=CARTESIAN_POINT('Origin',(0.,-1.,0.));
#23578=CARTESIAN_POINT('',(1.23627494547115,-1.,-1.81978687191668));
#23579=CARTESIAN_POINT('Ctrl Pts',(0.892032620296855,-1.,-1.5055822144029));
#23580=CARTESIAN_POINT('Ctrl Pts',(0.894452006964543,-1.,-1.50980486806688));
#23581=CARTESIAN_POINT('Ctrl Pts',(0.89918504748351,-1.,-1.51805569590094));
#23582=CARTESIAN_POINT('Ctrl Pts',(0.905967409625651,-1.,-1.52984849887993));
#23583=CARTESIAN_POINT('Ctrl Pts',(0.914375919026456,-1.,-1.54440491149498));
#23584=CARTESIAN_POINT('Ctrl Pts',(0.923832188944341,-1.,-1.56065988578893));
#23585=CARTESIAN_POINT('Ctrl Pts',(0.932246680108685,-1.,-1.57499388382243));
#23586=CARTESIAN_POINT('Ctrl Pts',(0.939646377893399,-1.,-1.58744937487176));
#23587=CARTESIAN_POINT('Ctrl Pts',(0.946078063315257,-1.,-1.59810042043673));
#23588=CARTESIAN_POINT('Ctrl Pts',(0.951613284356035,-1.,-1.60706069896936));
#23589=CARTESIAN_POINT('Ctrl Pts',(0.95635442292067,-1.,-1.61449324337085));
#23590=CARTESIAN_POINT('Ctrl Pts',(0.960438326101728,-1.,-1.62061638140221));
#23591=CARTESIAN_POINT('Ctrl Pts',(0.964046107040535,-1.,-1.62571930670187));
#23592=CARTESIAN_POINT('Ctrl Pts',(0.967387853230345,-1.,-1.63013849959462));
#23593=CARTESIAN_POINT('Ctrl Pts',(0.970669715997509,-1.,-1.63420665729798));
#23594=CARTESIAN_POINT('Ctrl Pts',(0.974066058287418,-1.,-1.63820952658144));
#23595=CARTESIAN_POINT('Ctrl Pts',(0.977689794119416,-1.,-1.64233990826687));
#23596=CARTESIAN_POINT('Ctrl Pts',(0.981562530939489,-1.,-1.64665139190656));
#23597=CARTESIAN_POINT('Ctrl Pts',(0.98564262292082,-1.,-1.65110016612638));
#23598=CARTESIAN_POINT('Ctrl Pts',(0.989855627854164,-1.,-1.65559044289699));
#23599=CARTESIAN_POINT('Ctrl Pts',(0.994121836661305,-1.,-1.66001553809947));
#23600=CARTESIAN_POINT('Ctrl Pts',(0.998389654952757,-1.,-1.66430758030376));
#23601=CARTESIAN_POINT('Ctrl Pts',(1.00265091003727,-1.,-1.66846059277303));
#23602=CARTESIAN_POINT('Ctrl Pts',(1.00692206696414,-1.,-1.67250335383293));
#23603=CARTESIAN_POINT('Ctrl Pts',(1.01123236493511,-1.,-1.67648246776464));
#23604=CARTESIAN_POINT('Ctrl Pts',(1.01561026162773,-1.,-1.68044289894798));
#23605=CARTESIAN_POINT('Ctrl Pts',(1.02006795074201,-1.,-1.68440578021706));
#23606=CARTESIAN_POINT('Ctrl Pts',(1.02460180535255,-1.,-1.68836910178447));
#23607=CARTESIAN_POINT('Ctrl Pts',(1.02919977579147,-1.,-1.69231840863458));
#23608=CARTESIAN_POINT('Ctrl Pts',(1.03384646003588,-1.,-1.69623414782771));
#23609=CARTESIAN_POINT('Ctrl Pts',(1.03852922490789,-1.,-1.70010052930962));
#23610=CARTESIAN_POINT('Ctrl Pts',(1.04324363334554,-1.,-1.70391338707982));
#23611=CARTESIAN_POINT('Ctrl Pts',(1.04799085404995,-1.,-1.70767646263649));
#23612=CARTESIAN_POINT('Ctrl Pts',(1.05277517202855,-1.,-1.71139783543989));
#23613=CARTESIAN_POINT('Ctrl Pts',(1.05760163192479,-1.,-1.7150865442702));
#23614=CARTESIAN_POINT('Ctrl Pts',(1.06247324680647,-1.,-1.71874858456904));
#23615=CARTESIAN_POINT('Ctrl Pts',(1.06738966975462,-1.,-1.72238500928453));
#23616=CARTESIAN_POINT('Ctrl Pts',(1.07234866990252,-1.,-1.72599406198488));
#23617=CARTESIAN_POINT('Ctrl Pts',(1.0773470373727,-1.,-1.72957248977424));
#23618=CARTESIAN_POINT('Ctrl Pts',(1.08238162784749,-1.,-1.73311705663407));
#23619=CARTESIAN_POINT('Ctrl Pts',(1.08745056285427,-1.,-1.73662628326091));
#23620=CARTESIAN_POINT('Ctrl Pts',(1.09255329056493,-1.,-1.74010053962247));
#23621=CARTESIAN_POINT('Ctrl Pts',(1.09768999241225,-1.,-1.74354119236208));
#23622=CARTESIAN_POINT('Ctrl Pts',(1.10286118991143,-1.,-1.74695004214923));
#23623=CARTESIAN_POINT('Ctrl Pts',(1.10806728183007,-1.,-1.7503286607592));
#23624=CARTESIAN_POINT('Ctrl Pts',(1.11330807582551,-1.,-1.7536777209463));
#23625=CARTESIAN_POINT('Ctrl Pts',(1.11858293216763,-1.,-1.75699720772105));
#23626=CARTESIAN_POINT('Ctrl Pts',(1.12389096855086,-1.,-1.76028671825096));
#23627=CARTESIAN_POINT('Ctrl Pts',(1.12923123555075,-1.,-1.7635457196617));
#23628=CARTESIAN_POINT('Ctrl Pts',(1.1346029180462,-1.,-1.76677384551862));
#23629=CARTESIAN_POINT('Ctrl Pts',(1.14000548336975,-1.,-1.76997111386769));
#23630=CARTESIAN_POINT('Ctrl Pts',(1.1454385822692,-1.,-1.77313777896194));
#23631=CARTESIAN_POINT('Ctrl Pts',(1.15090197841514,-1.,-1.7762742255701));
#23632=CARTESIAN_POINT('Ctrl Pts',(1.15639547194698,-1.,-1.77938085564275));
#23633=CARTESIAN_POINT('Ctrl Pts',(1.16191881298499,-1.,-1.78245795881009));
#23634=CARTESIAN_POINT('Ctrl Pts',(1.16747166312303,-1.,-1.78550566040443));
#23635=CARTESIAN_POINT('Ctrl Pts',(1.17305363177328,-1.,-1.78852398877617));
#23636=CARTESIAN_POINT('Ctrl Pts',(1.17866429440809,-1.,-1.79151291552689));
#23637=CARTESIAN_POINT('Ctrl Pts',(1.18430321697432,-1.,-1.79447240321515));
#23638=CARTESIAN_POINT('Ctrl Pts',(1.18996997934445,-1.,-1.79740245923478));
#23639=CARTESIAN_POINT('Ctrl Pts',(1.19566418930242,-1.,-1.80030314369879));
#23640=CARTESIAN_POINT('Ctrl Pts',(1.20138548938974,-1.,-1.80317454838603));
#23641=CARTESIAN_POINT('Ctrl Pts',(1.20713356605475,-1.,-1.80601678480707));
#23642=CARTESIAN_POINT('Ctrl Pts',(1.21290815708314,-1.,-1.80882996917129));
#23643=CARTESIAN_POINT('Ctrl Pts',(1.21870906103557,-1.,-1.81161420806656));
#23644=CARTESIAN_POINT('Ctrl Pts',(1.2245361330495,-1.,-1.81436959210434));
#23645=CARTESIAN_POINT('Ctrl Pts',(1.2292186489137,-1.,-1.8165508718364));
#23646=CARTESIAN_POINT('Ctrl Pts',(1.2327422452705,-1.,-1.81817389921279));
#23647=CARTESIAN_POINT('Ctrl Pts',(1.23509651170476,-1.,-1.81925017193666));
#23648=CARTESIAN_POINT('Ctrl Pts',(1.23627494547115,-1.,-1.81978687191668));
#23649=CARTESIAN_POINT('',(1.34869019493419,-1.,-1.73811241238545));
#23650=CARTESIAN_POINT('',(1.23627494547115,-1.,-1.81978687191668));
#23651=CARTESIAN_POINT('',(1.15624053661742,-1.,-1.31362392696032));
#23652=CARTESIAN_POINT('Ctrl Pts',(1.34869019493419,-1.,-1.73811241238545));
#23653=CARTESIAN_POINT('Ctrl Pts',(1.34854391898045,-1.,-1.73682580585691));
#23654=CARTESIAN_POINT('Ctrl Pts',(1.34824783112887,-1.,-1.73425417885907));
#23655=CARTESIAN_POINT('Ctrl Pts',(1.34779309152035,-1.,-1.7304014965394));
#23656=CARTESIAN_POINT('Ctrl Pts',(1.34716554819527,-1.,-1.72527410680674));
#23657=CARTESIAN_POINT('Ctrl Pts',(1.34634568653227,-1.,-1.7188807715049));
#23658=CARTESIAN_POINT('Ctrl Pts',(1.34549029589416,-1.,-1.71250340686822));
#23659=CARTESIAN_POINT('Ctrl Pts',(1.34459924533831,-1.,-1.70614212266738));
#23660=CARTESIAN_POINT('Ctrl Pts',(1.34367237124483,-1.,-1.69979707754427));
#23661=CARTESIAN_POINT('Ctrl Pts',(1.34270948206319,-1.,-1.6934684849687));
#23662=CARTESIAN_POINT('Ctrl Pts',(1.341710374848,-1.,-1.68715660868764));
#23663=CARTESIAN_POINT('Ctrl Pts',(1.34067485185203,-1.,-1.68086176030362));
#23664=CARTESIAN_POINT('Ctrl Pts',(1.3396027347034,-1.,-1.67458429426086));
#23665=CARTESIAN_POINT('Ctrl Pts',(1.33849388654388,-1.,-1.66832460783989));
#23666=CARTESIAN_POINT('Ctrl Pts',(1.33734820885262,-1.,-1.66208312541983));
#23667=CARTESIAN_POINT('Ctrl Pts',(1.33616559745172,-1.,-1.65586025952593));
#23668=CARTESIAN_POINT('Ctrl Pts',(1.33494590467993,-1.,-1.6496563728683));
#23669=CARTESIAN_POINT('Ctrl Pts',(1.33368890676572,-1.,-1.6434717485603));
#23670=CARTESIAN_POINT('Ctrl Pts',(1.33239425103724,-1.,-1.63730653475089));
#23671=CARTESIAN_POINT('Ctrl Pts',(1.33106149345645,-1.,-1.63116079730923));
#23672=CARTESIAN_POINT('Ctrl Pts',(1.3296901950568,-1.,-1.62503464209797));
#23673=CARTESIAN_POINT('Ctrl Pts',(1.32828000610449,-1.,-1.61892832270724));
#23674=CARTESIAN_POINT('Ctrl Pts',(1.32683074483356,-1.,-1.6128423401575));
#23675=CARTESIAN_POINT('Ctrl Pts',(1.32534250785782,-1.,-1.60677758290954));
#23676=CARTESIAN_POINT('Ctrl Pts',(1.32381550858256,-1.,-1.60073511858687));
#23677=CARTESIAN_POINT('Ctrl Pts',(1.32224985747682,-1.,-1.59471591079403));
#23678=CARTESIAN_POINT('Ctrl Pts',(1.32064537110892,-1.,-1.58872057258245));
#23679=CARTESIAN_POINT('Ctrl Pts',(1.31900135021432,-1.,-1.58274907898834));
#23680=CARTESIAN_POINT('Ctrl Pts',(1.31731642317187,-1.,-1.5768005650559));
#23681=CARTESIAN_POINT('Ctrl Pts',(1.31558903860016,-1.,-1.57087397835723));
#23682=CARTESIAN_POINT('Ctrl Pts',(1.31381795281002,-1.,-1.56496872402353));
#23683=CARTESIAN_POINT('Ctrl Pts',(1.31200264341696,-1.,-1.55908521254821));
#23684=CARTESIAN_POINT('Ctrl Pts',(1.31014393684222,-1.,-1.55322568759481));
#23685=CARTESIAN_POINT('Ctrl Pts',(1.30824393907473,-1.,-1.54739413957185));
#23686=CARTESIAN_POINT('Ctrl Pts',(1.30630475189556,-1.,-1.54159462645432));
#23687=CARTESIAN_POINT('Ctrl Pts',(1.30432735639489,-1.,-1.53582981268977));
#23688=CARTESIAN_POINT('Ctrl Pts',(1.30231064395568,-1.,-1.53009970283891));
#23689=CARTESIAN_POINT('Ctrl Pts',(1.30024984366328,-1.,-1.52439957861062));
#23690=CARTESIAN_POINT('Ctrl Pts',(1.29813791800747,-1.,-1.51872184912724));
#23691=CARTESIAN_POINT('Ctrl Pts',(1.29596850710509,-1.,-1.51305994241402));
#23692=CARTESIAN_POINT('Ctrl Pts',(1.29373841372842,-1.,-1.50741159078365));
#23693=CARTESIAN_POINT('Ctrl Pts',(1.29145022885181,-1.,-1.50178230149776));
#23694=CARTESIAN_POINT('Ctrl Pts',(1.28911506584254,-1.,-1.49618896881754));
#23695=CARTESIAN_POINT('Ctrl Pts',(1.2867467611644,-1.,-1.4906522831278));
#23696=CARTESIAN_POINT('Ctrl Pts',(1.28435533880201,-1.,-1.4851881711891));
#23697=CARTESIAN_POINT('Ctrl Pts',(1.28194158939517,-1.,-1.47980070347096));
#23698=CARTESIAN_POINT('Ctrl Pts',(1.2794891824849,-1.,-1.4744717526707));
#23699=CARTESIAN_POINT('Ctrl Pts',(1.27696414831089,-1.,-1.46916035917133));
#23700=CARTESIAN_POINT('Ctrl Pts',(1.27433119897822,-1.,-1.46382431332476));
#23701=CARTESIAN_POINT('Ctrl Pts',(1.27156805265289,-1.,-1.45843906294697));
#23702=CARTESIAN_POINT('Ctrl Pts',(1.2686778680489,-1.,-1.45301422764247));
#23703=CARTESIAN_POINT('Ctrl Pts',(1.26570925118868,-1.,-1.44761985001662));
#23704=CARTESIAN_POINT('Ctrl Pts',(1.26273903323858,-1.,-1.44236470511303));
#23705=CARTESIAN_POINT('Ctrl Pts',(1.25983531012005,-1.,-1.43734919180848));
#23706=CARTESIAN_POINT('Ctrl Pts',(1.25702687965755,-1.,-1.43262645609691));
#23707=CARTESIAN_POINT('Ctrl Pts',(1.25426945222639,-1.,-1.42815938799387));
#23708=CARTESIAN_POINT('Ctrl Pts',(1.2514145557001,-1.,-1.42378102115575));
#23709=CARTESIAN_POINT('Ctrl Pts',(1.24824430986571,-1.,-1.41923722596025));
#23710=CARTESIAN_POINT('Ctrl Pts',(1.24450600513056,-1.,-1.41422913175179));
#23711=CARTESIAN_POINT('Ctrl Pts',(1.23994455029534,-1.,-1.40845295531283));
#23712=CARTESIAN_POINT('Ctrl Pts',(1.23434087290423,-1.,-1.40164708206106));
#23713=CARTESIAN_POINT('Ctrl Pts',(1.22752961899387,-1.,-1.39361389568796));
#23714=CARTESIAN_POINT('Ctrl Pts',(1.21938737280852,-1.,-1.38420564527715));
#23715=CARTESIAN_POINT('Ctrl Pts',(1.20982812925645,-1.,-1.37331915607905));
#23716=CARTESIAN_POINT('Ctrl Pts',(1.1987959077932,-1.,-1.36088705043885));
#23717=CARTESIAN_POINT('Ctrl Pts',(1.18625865667441,-1.,-1.34687054001093));
#23718=CARTESIAN_POINT('Ctrl Pts',(1.17501305789857,-1.,-1.33437539347008));
#23719=CARTESIAN_POINT('Ctrl Pts',(1.16589330093588,-1.,-1.32428080721772));
#23720=CARTESIAN_POINT('Ctrl Pts',(1.15950888730809,-1.,-1.31722977216397));
#23721=CARTESIAN_POINT('Ctrl Pts',(1.15624053661742,-1.,-1.31362392696032));
#23722=CARTESIAN_POINT('',(1.31362392696032,-1.,-1.15624053661742));
#23723=CARTESIAN_POINT('Origin',(0.,-1.,0.));
#23724=CARTESIAN_POINT('',(1.73811241238545,-1.,-1.34869019493419));
#23725=CARTESIAN_POINT('Ctrl Pts',(1.31362392696032,-1.,-1.15624053661742));
#23726=CARTESIAN_POINT('Ctrl Pts',(1.3172297721596,-1.,-1.15950888730433));
#23727=CARTESIAN_POINT('Ctrl Pts',(1.32428080720544,-1.,-1.16589330092532));
#23728=CARTESIAN_POINT('Ctrl Pts',(1.33437539344842,-1.,-1.17501305787994));
#23729=CARTESIAN_POINT('Ctrl Pts',(1.34687053998157,-1.,-1.18625865664915));
#23730=CARTESIAN_POINT('Ctrl Pts',(1.36088705040677,-1.,-1.1987959077656));
#23731=CARTESIAN_POINT('Ctrl Pts',(1.37331915604962,-1.,-1.20982812923113));
#23732=CARTESIAN_POINT('Ctrl Pts',(1.38420564525391,-1.,-1.21938737278853));
#23733=CARTESIAN_POINT('Ctrl Pts',(1.39361389567257,-1.,-1.22752961898063));
#23734=CARTESIAN_POINT('Ctrl Pts',(1.40164708205345,-1.,-1.23434087289768));
#23735=CARTESIAN_POINT('Ctrl Pts',(1.40845295531151,-1.,-1.23994455029421));
#23736=CARTESIAN_POINT('Ctrl Pts',(1.41422913175437,-1.,-1.24450600513278));
#23737=CARTESIAN_POINT('Ctrl Pts',(1.41923722596421,-1.,-1.24824430986911));
#23738=CARTESIAN_POINT('Ctrl Pts',(1.42378102115911,-1.,-1.25141455570299));
#23739=CARTESIAN_POINT('Ctrl Pts',(1.42815938799555,-1.,-1.25426945222783));
#23740=CARTESIAN_POINT('Ctrl Pts',(1.43262645609679,-1.,-1.25702687965744));
#23741=CARTESIAN_POINT('Ctrl Pts',(1.43734919180719,-1.,-1.25983531011894));
#23742=CARTESIAN_POINT('Ctrl Pts',(1.44236470511145,-1.,-1.26273903323723));
#23743=CARTESIAN_POINT('Ctrl Pts',(1.44761985001544,-1.,-1.26570925118767));
#23744=CARTESIAN_POINT('Ctrl Pts',(1.45301422764205,-1.,-1.26867786804854));
#23745=CARTESIAN_POINT('Ctrl Pts',(1.45843906294725,-1.,-1.27156805265312));
#23746=CARTESIAN_POINT('Ctrl Pts',(1.4638243133254,-1.,-1.27433119897877));
#23747=CARTESIAN_POINT('Ctrl Pts',(1.46916035917197,-1.,-1.27696414831144));
#23748=CARTESIAN_POINT('Ctrl Pts',(1.4744717526711,-1.,-1.27948918248524));
#23749=CARTESIAN_POINT('Ctrl Pts',(1.47980070347102,-1.,-1.28194158939522));
#23750=CARTESIAN_POINT('Ctrl Pts',(1.48518817118891,-1.,-1.28435533880184));
#23751=CARTESIAN_POINT('Ctrl Pts',(1.4906522831275,-1.,-1.28674676116415));
#23752=CARTESIAN_POINT('Ctrl Pts',(1.49618896881729,-1.,-1.28911506584232));
#23753=CARTESIAN_POINT('Ctrl Pts',(1.50178230149764,-1.,-1.29145022885171));
#23754=CARTESIAN_POINT('Ctrl Pts',(1.50741159078367,-1.,-1.29373841372843));
#23755=CARTESIAN_POINT('Ctrl Pts',(1.51305994241412,-1.,-1.29596850710518));
#23756=CARTESIAN_POINT('Ctrl Pts',(1.51872184912735,-1.,-1.29813791800757));
#23757=CARTESIAN_POINT('Ctrl Pts',(1.5243995786107,-1.,-1.30024984366334));
#23758=CARTESIAN_POINT('Ctrl Pts',(1.53009970283893,-1.,-1.3023106439557));
#23759=CARTESIAN_POINT('Ctrl Pts',(1.53582981268976,-1.,-1.30432735639487));
#23760=CARTESIAN_POINT('Ctrl Pts',(1.54159462645428,-1.,-1.30630475189553));
#23761=CARTESIAN_POINT('Ctrl Pts',(1.54739413957183,-1.,-1.30824393907471));
#23762=CARTESIAN_POINT('Ctrl Pts',(1.55322568759481,-1.,-1.31014393684221));
#23763=CARTESIAN_POINT('Ctrl Pts',(1.55908521254822,-1.,-1.31200264341696));
#23764=CARTESIAN_POINT('Ctrl Pts',(1.56496872402352,-1.,-1.31381795281002));
#23765=CARTESIAN_POINT('Ctrl Pts',(1.57087397835721,-1.,-1.31558903860015));
#23766=CARTESIAN_POINT('Ctrl Pts',(1.57680056505585,-1.,-1.31731642317183));
#23767=CARTESIAN_POINT('Ctrl Pts',(1.58274907898829,-1.,-1.31900135021428));
#23768=CARTESIAN_POINT('Ctrl Pts',(1.58872057258244,-1.,-1.32064537110891));
#23769=CARTESIAN_POINT('Ctrl Pts',(1.59471591079408,-1.,-1.32224985747686));
#23770=CARTESIAN_POINT('Ctrl Pts',(1.600735118587,-1.,-1.32381550858266));
#23771=CARTESIAN_POINT('Ctrl Pts',(1.6067775829097,-1.,-1.32534250785794));
#23772=CARTESIAN_POINT('Ctrl Pts',(1.61284234015762,-1.,-1.32683074483365));
#23773=CARTESIAN_POINT('Ctrl Pts',(1.61892832270723,-1.,-1.32828000610448));
#23774=CARTESIAN_POINT('Ctrl Pts',(1.62503464209777,-1.,-1.32969019505665));
#23775=CARTESIAN_POINT('Ctrl Pts',(1.63116079730887,-1.,-1.33106149345618));
#23776=CARTESIAN_POINT('Ctrl Pts',(1.63730653475049,-1.,-1.33239425103694));
#23777=CARTESIAN_POINT('Ctrl Pts',(1.64347174856007,-1.,-1.33368890676554));
#23778=CARTESIAN_POINT('Ctrl Pts',(1.64965637286843,-1.,-1.33494590468003));
#23779=CARTESIAN_POINT('Ctrl Pts',(1.65586025952651,-1.,-1.33616559745217));
#23780=CARTESIAN_POINT('Ctrl Pts',(1.66208312542073,-1.,-1.33734820885331));
#23781=CARTESIAN_POINT('Ctrl Pts',(1.66832460784078,-1.,-1.33849388654458));
#23782=CARTESIAN_POINT('Ctrl Pts',(1.67458429426126,-1.,-1.33960273470372));
#23783=CARTESIAN_POINT('Ctrl Pts',(1.68086176030308,-1.,-1.3406748518516));
#23784=CARTESIAN_POINT('Ctrl Pts',(1.68715660868602,-1.,-1.34171037484673));
#23785=CARTESIAN_POINT('Ctrl Pts',(1.6934684849664,-1.,-1.34270948206139));
#23786=CARTESIAN_POINT('Ctrl Pts',(1.69979707754221,-1.,-1.34367237124322));
#23787=CARTESIAN_POINT('Ctrl Pts',(1.70614212266676,-1.,-1.34459924533783));
#23788=CARTESIAN_POINT('Ctrl Pts',(1.71250340687011,-1.,-1.34549029589563));
#23789=CARTESIAN_POINT('Ctrl Pts',(1.7188807715095,-1.,-1.34634568653586));
#23790=CARTESIAN_POINT('Ctrl Pts',(1.72527410681298,-1.,-1.34716554820013));
#23791=CARTESIAN_POINT('Ctrl Pts',(1.73040149654497,-1.,-1.3477930915247));
#23792=CARTESIAN_POINT('Ctrl Pts',(1.73425417886254,-1.,-1.34824783113158));
#23793=CARTESIAN_POINT('Ctrl Pts',(1.73682580585819,-1.,-1.34854391898145));
#23794=CARTESIAN_POINT('Ctrl Pts',(1.73811241238545,-1.,-1.34869019493419));
#23795=CARTESIAN_POINT('',(1.81978687191668,-1.,-1.23627494547115));
#23796=CARTESIAN_POINT('',(1.73811241238545,-1.,-1.34869019493419));
#23797=CARTESIAN_POINT('',(1.5055822144029,-1.,-0.892032620296855));
#23798=CARTESIAN_POINT('Ctrl Pts',(1.81978687191668,-1.,-1.23627494547115));
#23799=CARTESIAN_POINT('Ctrl Pts',(1.81925017193531,-1.,-1.23509651170384));
#23800=CARTESIAN_POINT('Ctrl Pts',(1.81817389920914,-1.,-1.23274224526804));
#23801=CARTESIAN_POINT('Ctrl Pts',(1.81655087183054,-1.,-1.22921864890975));
#23802=CARTESIAN_POINT('Ctrl Pts',(1.81436959209778,-1.,-1.22453613304507));
#23803=CARTESIAN_POINT('Ctrl Pts',(1.81161420806172,-1.,-1.2187090610323));
#23804=CARTESIAN_POINT('Ctrl Pts',(1.80882996916931,-1.,-1.2129081570818));
#23805=CARTESIAN_POINT('Ctrl Pts',(1.80601678480772,-1.,-1.20713356605519));
#23806=CARTESIAN_POINT('Ctrl Pts',(1.8031745483882,-1.,-1.2013854893912));
#23807=CARTESIAN_POINT('Ctrl Pts',(1.80030314370121,-1.,-1.19566418930405));
#23808=CARTESIAN_POINT('Ctrl Pts',(1.79740245923649,-1.,-1.1899699793456));
#23809=CARTESIAN_POINT('Ctrl Pts',(1.79447240321572,-1.,-1.18430321697471));
#23810=CARTESIAN_POINT('Ctrl Pts',(1.79151291552646,-1.,-1.17866429440781));
#23811=CARTESIAN_POINT('Ctrl Pts',(1.78852398877523,-1.,-1.17305363177265));
#23812=CARTESIAN_POINT('Ctrl Pts',(1.78550566040349,-1.,-1.16747166312239));
#23813=CARTESIAN_POINT('Ctrl Pts',(1.78245795880949,-1.,-1.16191881298458));
#23814=CARTESIAN_POINT('Ctrl Pts',(1.77938085564261,-1.,-1.15639547194689));
#23815=CARTESIAN_POINT('Ctrl Pts',(1.77627422557034,-1.,-1.15090197841531));
#23816=CARTESIAN_POINT('Ctrl Pts',(1.77313777896234,-1.,-1.14543858226948));
#23817=CARTESIAN_POINT('Ctrl Pts',(1.76997111386806,-1.,-1.14000548337));
#23818=CARTESIAN_POINT('Ctrl Pts',(1.76677384551883,-1.,-1.13460291804635));
#23819=CARTESIAN_POINT('Ctrl Pts',(1.76354571966171,-1.,-1.12923123555076));
#23820=CARTESIAN_POINT('Ctrl Pts',(1.76028671825084,-1.,-1.12389096855078));
#23821=CARTESIAN_POINT('Ctrl Pts',(1.75699720772089,-1.,-1.11858293216752));
#23822=CARTESIAN_POINT('Ctrl Pts',(1.75367772094617,-1.,-1.11330807582542));
#23823=CARTESIAN_POINT('Ctrl Pts',(1.75032866075914,-1.,-1.10806728183003));
#23824=CARTESIAN_POINT('Ctrl Pts',(1.74695004214924,-1.,-1.10286118991144));
#23825=CARTESIAN_POINT('Ctrl Pts',(1.74354119236212,-1.,-1.09768999241229));
#23826=CARTESIAN_POINT('Ctrl Pts',(1.74010053962252,-1.,-1.09255329056496));
#23827=CARTESIAN_POINT('Ctrl Pts',(1.73662628326093,-1.,-1.08745056285429));
#23828=CARTESIAN_POINT('Ctrl Pts',(1.73311705663407,-1.,-1.08238162784749));
#23829=CARTESIAN_POINT('Ctrl Pts',(1.72957248977424,-1.,-1.0773470373727));
#23830=CARTESIAN_POINT('Ctrl Pts',(1.72599406198489,-1.,-1.07234866990252));
#23831=CARTESIAN_POINT('Ctrl Pts',(1.72238500928456,-1.,-1.06738966975463));
#23832=CARTESIAN_POINT('Ctrl Pts',(1.71874858456908,-1.,-1.0624732468065));
#23833=CARTESIAN_POINT('Ctrl Pts',(1.71508654427022,-1.,-1.05760163192481));
#23834=CARTESIAN_POINT('Ctrl Pts',(1.71139783543986,-1.,-1.05277517202854));
#23835=CARTESIAN_POINT('Ctrl Pts',(1.70767646263641,-1.,-1.0479908540499));
#23836=CARTESIAN_POINT('Ctrl Pts',(1.70391338707969,-1.,-1.04324363334546));
#23837=CARTESIAN_POINT('Ctrl Pts',(1.70010052930951,-1.,-1.03852922490782));
#23838=CARTESIAN_POINT('Ctrl Pts',(1.69623414782769,-1.,-1.03384646003587));
#23839=CARTESIAN_POINT('Ctrl Pts',(1.69231840863471,-1.,-1.02919977579155));
#23840=CARTESIAN_POINT('Ctrl Pts',(1.68836910178475,-1.,-1.02460180535272));
#23841=CARTESIAN_POINT('Ctrl Pts',(1.68440578021739,-1.,-1.02006795074222));
#23842=CARTESIAN_POINT('Ctrl Pts',(1.6804428989482,-1.,-1.01561026162787));
#23843=CARTESIAN_POINT('Ctrl Pts',(1.67648246776457,-1.,-1.01123236493507));
#23844=CARTESIAN_POINT('Ctrl Pts',(1.67250335383248,-1.,-1.00692206696387));
#23845=CARTESIAN_POINT('Ctrl Pts',(1.66846059277231,-1.,-1.00265091003682));
#23846=CARTESIAN_POINT('Ctrl Pts',(1.66430758030304,-1.,-0.998389654952317));
#23847=CARTESIAN_POINT('Ctrl Pts',(1.66001553809916,-1.,-0.994121836661116));
#23848=CARTESIAN_POINT('Ctrl Pts',(1.65559044289746,-1.,-0.98985562785445));
#23849=CARTESIAN_POINT('Ctrl Pts',(1.6511001661277,-1.,-0.985642622921626));
#23850=CARTESIAN_POINT('Ctrl Pts',(1.64665139190834,-1.,-0.981562530940574));
#23851=CARTESIAN_POINT('Ctrl Pts',(1.64233990826831,-1.,-0.977689794120297));
#23852=CARTESIAN_POINT('Ctrl Pts',(1.63820952658157,-1.,-0.974066058287501));
#23853=CARTESIAN_POINT('Ctrl Pts',(1.63420665729609,-1.,-0.970669715996356));
#23854=CARTESIAN_POINT('Ctrl Pts',(1.63013849959083,-1.,-0.967387853228041));
#23855=CARTESIAN_POINT('Ctrl Pts',(1.6257193066974,-1.,-0.964046107037821));
#23856=CARTESIAN_POINT('Ctrl Pts',(1.62061638139929,-1.,-0.960438326099958));
#23857=CARTESIAN_POINT('Ctrl Pts',(1.61449324337233,-1.,-0.956354422921573));
#23858=CARTESIAN_POINT('Ctrl Pts',(1.60706069897794,-1.,-0.951613284361248));
#23859=CARTESIAN_POINT('Ctrl Pts',(1.59810042045408,-1.,-0.946078063325796));
#23860=CARTESIAN_POINT('Ctrl Pts',(1.58744937489796,-1.,-0.939646377909319));
#23861=CARTESIAN_POINT('Ctrl Pts',(1.57499388385561,-1.,-0.932246680128849));
#23862=CARTESIAN_POINT('Ctrl Pts',(1.56065988582509,-1.,-0.923832188966322));
#23863=CARTESIAN_POINT('Ctrl Pts',(1.54440491152807,-1.,-0.91437591904658));
#23864=CARTESIAN_POINT('Ctrl Pts',(1.52984849890434,-1.,-0.905967409640499));
#23865=CARTESIAN_POINT('Ctrl Pts',(1.51805569591479,-1.,-0.89918504749193));
#23866=CARTESIAN_POINT('Ctrl Pts',(1.50980486807181,-1.,-0.894452006967538));
#23867=CARTESIAN_POINT('Ctrl Pts',(1.5055822144029,-1.,-0.892032620296855));
#23868=CARTESIAN_POINT('',(1.60662857109684,-1.,-0.693717979106306));
#23869=CARTESIAN_POINT('Origin',(0.,-1.,0.));
#23870=CARTESIAN_POINT('',(2.0698113262342,-1.,-0.745574324794401));
#23871=CARTESIAN_POINT('Ctrl Pts',(1.60662857109684,-1.,-0.693717979106306));
#23872=CARTESIAN_POINT('Ctrl Pts',(1.61106790957619,-1.,-0.69571209787897));
#23873=CARTESIAN_POINT('Ctrl Pts',(1.61974673471117,-1.,-0.699605146398837));
#23874=CARTESIAN_POINT('Ctrl Pts',(1.6321654166204,-1.,-0.705159151977294));
#23875=CARTESIAN_POINT('Ctrl Pts',(1.64752408828442,-1.,-0.711993139340448));
#23876=CARTESIAN_POINT('Ctrl Pts',(1.66472880551777,-1.,-0.71958543378795));
#23877=CARTESIAN_POINT('Ctrl Pts',(1.67996158451922,-1.,-0.726235967982445));
#23878=CARTESIAN_POINT('Ctrl Pts',(1.69326921972915,-1.,-0.731963238685357));
#23879=CARTESIAN_POINT('Ctrl Pts',(1.70473309004249,-1.,-0.736799665716932));
#23880=CARTESIAN_POINT('Ctrl Pts',(1.71447789751001,-1.,-0.74079516202821));
#23881=CARTESIAN_POINT('Ctrl Pts',(1.72268229916769,-1.,-0.744021445433094));
#23882=CARTESIAN_POINT('Ctrl Pts',(1.72958533647714,-1.,-0.746574710097752));
#23883=CARTESIAN_POINT('Ctrl Pts',(1.7355035168033,-1.,-0.74858246295687));
#23884=CARTESIAN_POINT('Ctrl Pts',(1.74080458267114,-1.,-0.75019343598125));
#23885=CARTESIAN_POINT('Ctrl Pts',(1.74585086852502,-1.,-0.751555614164483));
#23886=CARTESIAN_POINT('Ctrl Pts',(1.75095139468794,-1.,-0.752797683531314));
#23887=CARTESIAN_POINT('Ctrl Pts',(1.75631083600019,-1.,-0.754009254027829));
#23888=CARTESIAN_POINT('Ctrl Pts',(1.76197817240128,-1.,-0.755220979974462));
#23889=CARTESIAN_POINT('Ctrl Pts',(1.76789396002998,-1.,-0.75642189602781));
#23890=CARTESIAN_POINT('Ctrl Pts',(1.77394167108292,-1.,-0.757578264077029));
#23891=CARTESIAN_POINT('Ctrl Pts',(1.77999411220945,-1.,-0.758650626677519));
#23892=CARTESIAN_POINT('Ctrl Pts',(1.78596964884604,-1.,-0.75961440111019));
#23893=CARTESIAN_POINT('Ctrl Pts',(1.7918581561088,-1.,-0.760469555880749));
#23894=CARTESIAN_POINT('Ctrl Pts',(1.79768986997783,-1.,-0.761229695230558));
#23895=CARTESIAN_POINT('Ctrl Pts',(1.80351583877342,-1.,-0.761915336443547));
#23896=CARTESIAN_POINT('Ctrl Pts',(1.80938551463965,-1.,-0.762546129463938));
#23897=CARTESIAN_POINT('Ctrl Pts',(1.8153211840553,-1.,-0.763132003836634));
#23898=CARTESIAN_POINT('Ctrl Pts',(1.82131873145266,-1.,-0.763673465462727));
#23899=CARTESIAN_POINT('Ctrl Pts',(1.82735991200065,-1.,-0.764165902605995));
#23900=CARTESIAN_POINT('Ctrl Pts',(1.83342077227142,-1.,-0.764602549687853));
#23901=CARTESIAN_POINT('Ctrl Pts',(1.83948181064835,-1.,-0.764978057881738));
#23902=CARTESIAN_POINT('Ctrl Pts',(1.84553698875924,-1.,-0.765291664862029));
#23903=CARTESIAN_POINT('Ctrl Pts',(1.85158945130063,-1.,-0.765545710619063));
#23904=CARTESIAN_POINT('Ctrl Pts',(1.85764741390394,-1.,-0.765744212909319));
#23905=CARTESIAN_POINT('Ctrl Pts',(1.86372027063312,-1.,-0.765891519092547));
#23906=CARTESIAN_POINT('Ctrl Pts',(1.86981398314341,-1.,-0.765990708546091));
#23907=CARTESIAN_POINT('Ctrl Pts',(1.87592888967883,-1.,-0.766042837036744));
#23908=CARTESIAN_POINT('Ctrl Pts',(1.88206215302561,-1.,-0.766047794851865));
#23909=CARTESIAN_POINT('Ctrl Pts',(1.88820926433409,-1.,-0.766004837062091));
#23910=CARTESIAN_POINT('Ctrl Pts',(1.89436577771388,-1.,-0.765913193856978));
#23911=CARTESIAN_POINT('Ctrl Pts',(1.90052930393596,-1.,-0.765772772593386));
#23912=CARTESIAN_POINT('Ctrl Pts',(1.90669961402356,-1.,-0.765584196937919));
#23913=CARTESIAN_POINT('Ctrl Pts',(1.91287765805169,-1.,-0.765348465884722));
#23914=CARTESIAN_POINT('Ctrl Pts',(1.91906491634196,-1.,-0.765066729667089));
#23915=CARTESIAN_POINT('Ctrl Pts',(1.92526263537048,-1.,-0.764740025488212));
#23916=CARTESIAN_POINT('Ctrl Pts',(1.93147105496382,-1.,-0.764369010673941));
#23917=CARTESIAN_POINT('Ctrl Pts',(1.93768964875886,-1.,-0.763954049121459));
#23918=CARTESIAN_POINT('Ctrl Pts',(1.9439174661764,-1.,-0.763495333538629));
#23919=CARTESIAN_POINT('Ctrl Pts',(1.95015342590024,-1.,-0.762992990878769));
#23920=CARTESIAN_POINT('Ctrl Pts',(1.95639665309869,-1.,-0.762447203806179));
#23921=CARTESIAN_POINT('Ctrl Pts',(1.96264672744186,-1.,-0.761858300014424));
#23922=CARTESIAN_POINT('Ctrl Pts',(1.96890351582499,-1.,-0.761226690483821));
#23923=CARTESIAN_POINT('Ctrl Pts',(1.97516705321494,-1.,-0.760552825409757));
#23924=CARTESIAN_POINT('Ctrl Pts',(1.98143741418172,-1.,-0.75983714745219));
#23925=CARTESIAN_POINT('Ctrl Pts',(1.98771456680874,-1.,-0.759080037802488));
#23926=CARTESIAN_POINT('Ctrl Pts',(1.99399831098817,-1.,-0.758281796766761));
#23927=CARTESIAN_POINT('Ctrl Pts',(2.00028834739178,-1.,-0.757442676862724));
#23928=CARTESIAN_POINT('Ctrl Pts',(2.0065843158773,-1.,-0.756562904646671));
#23929=CARTESIAN_POINT('Ctrl Pts',(2.01288584328084,-1.,-0.755642704957865));
#23930=CARTESIAN_POINT('Ctrl Pts',(2.01919259405809,-1.,-0.754682330722816));
#23931=CARTESIAN_POINT('Ctrl Pts',(2.02550428623313,-1.,-0.753682061112768));
#23932=CARTESIAN_POINT('Ctrl Pts',(2.03182068456221,-1.,-0.752642180487211));
#23933=CARTESIAN_POINT('Ctrl Pts',(2.03814160092099,-1.,-0.751562963361115));
#23934=CARTESIAN_POINT('Ctrl Pts',(2.04446689147979,-1.,-0.750444657875576));
#23935=CARTESIAN_POINT('Ctrl Pts',(2.05079645592154,-1.,-0.749287468665046));
#23936=CARTESIAN_POINT('Ctrl Pts',(2.05713023031006,-1.,-0.748091554183803));
#23937=CARTESIAN_POINT('Ctrl Pts',(2.06220058927826,-1.,-0.74710393278792));
#23938=CARTESIAN_POINT('Ctrl Pts',(2.06600523016815,-1.,-0.746345871544201));
#23939=CARTESIAN_POINT('Ctrl Pts',(2.06854248895728,-1.,-0.745832791378367));
#23940=CARTESIAN_POINT('Ctrl Pts',(2.0698113262342,-1.,-0.745574324794401));
#23941=CARTESIAN_POINT('',(2.11275013067528,-1.,-0.61342227326009));
#23942=CARTESIAN_POINT('',(2.0698113262342,-1.,-0.745574324794401));
#23943=CARTESIAN_POINT('',(1.7075470150345,-1.,-0.383122945602004));
#23944=CARTESIAN_POINT('Ctrl Pts',(2.11275013067528,-1.,-0.61342227326009));
#23945=CARTESIAN_POINT('Ctrl Pts',(2.11187554259986,-1.,-0.6124673655618));
#23946=CARTESIAN_POINT('Ctrl Pts',(2.11012443807238,-1.,-0.610560911689899));
#23947=CARTESIAN_POINT('Ctrl Pts',(2.1074919961518,-1.,-0.607711315454876));
#23948=CARTESIAN_POINT('Ctrl Pts',(2.10397049886949,-1.,-0.60393203073603));
#23949=CARTESIAN_POINT('Ctrl Pts',(2.0995493086477,-1.,-0.599241616420534));
#23950=CARTESIAN_POINT('Ctrl Pts',(2.0951087622027,-1.,-0.594585006052162));
#23951=CARTESIAN_POINT('Ctrl Pts',(2.09064881812129,-1.,-0.589962365403406));
#23952=CARTESIAN_POINT('Ctrl Pts',(2.08616943727951,-1.,-0.585373918991617));
#23953=CARTESIAN_POINT('Ctrl Pts',(2.08167059018418,-1.,-0.580819952108064));
#23954=CARTESIAN_POINT('Ctrl Pts',(2.07715226767559,-1.,-0.576300797416845));
#23955=CARTESIAN_POINT('Ctrl Pts',(2.07261449292824,-1.,-0.571816823242603));
#23956=CARTESIAN_POINT('Ctrl Pts',(2.06805732997334,-1.,-0.567368421181087));
#23957=CARTESIAN_POINT('Ctrl Pts',(2.06348090160589,-1.,-0.562955993082262));
#23958=CARTESIAN_POINT('Ctrl Pts',(2.05888537756462,-1.,-0.558579940185152));
#23959=CARTESIAN_POINT('Ctrl Pts',(2.05427091604413,-1.,-0.554240657463906));
#23960=CARTESIAN_POINT('Ctrl Pts',(2.04963761077958,-1.,-0.549938525150295));
#23961=CARTESIAN_POINT('Ctrl Pts',(2.04498544714588,-1.,-0.54567390381743));
#23962=CARTESIAN_POINT('Ctrl Pts',(2.04031422690527,-1.,-0.541447120615659));
#23963=CARTESIAN_POINT('Ctrl Pts',(2.03562362954037,-1.,-0.537258489833262));
#23964=CARTESIAN_POINT('Ctrl Pts',(2.03091336214426,-1.,-0.533108355132977));
#23965=CARTESIAN_POINT('Ctrl Pts',(2.0261832908329,-1.,-0.528997127241914));
#23966=CARTESIAN_POINT('Ctrl Pts',(2.02143356304698,-1.,-0.524925318333476));
#23967=CARTESIAN_POINT('Ctrl Pts',(2.01666477917286,-1.,-0.520893590399371));
#23968=CARTESIAN_POINT('Ctrl Pts',(2.01187773939242,-1.,-0.516902681728687));
#23969=CARTESIAN_POINT('Ctrl Pts',(2.00707309946949,-1.,-0.512953306961793));
#23970=CARTESIAN_POINT('Ctrl Pts',(2.00225107134734,-1.,-0.509046069886157));
#23971=CARTESIAN_POINT('Ctrl Pts',(1.99741107463572,-1.,-0.505181361323026));
#23972=CARTESIAN_POINT('Ctrl Pts',(1.99255149126155,-1.,-0.501359287727146));
#23973=CARTESIAN_POINT('Ctrl Pts',(1.98767044752932,-1.,-0.497579909545574));
#23974=CARTESIAN_POINT('Ctrl Pts',(1.98276658761821,-1.,-0.493843476541495));
#23975=CARTESIAN_POINT('Ctrl Pts',(1.97783973019229,-1.,-0.490150627860953));
#23976=CARTESIAN_POINT('Ctrl Pts',(1.97289186263272,-1.,-0.486502692907659));
#23977=CARTESIAN_POINT('Ctrl Pts',(1.96792703422362,-1.,-0.482901662120691));
#23978=CARTESIAN_POINT('Ctrl Pts',(1.96294933055943,-1.,-0.479349583074855));
#23979=CARTESIAN_POINT('Ctrl Pts',(1.95796111148177,-1.,-0.475848034683176));
#23980=CARTESIAN_POINT('Ctrl Pts',(1.95296148278133,-1.,-0.472397672264072));
#23981=CARTESIAN_POINT('Ctrl Pts',(1.94794381136514,-1.,-0.468997482913135));
#23982=CARTESIAN_POINT('Ctrl Pts',(1.9428979419619,-1.,-0.46564546202603));
#23983=CARTESIAN_POINT('Ctrl Pts',(1.93781486640821,-1.,-0.462340031009057));
#23984=CARTESIAN_POINT('Ctrl Pts',(1.93269066517934,-1.,-0.459081234547926));
#23985=CARTESIAN_POINT('Ctrl Pts',(1.92753067150476,-1.,-0.455872005174371));
#23986=CARTESIAN_POINT('Ctrl Pts',(1.92235380648502,-1.,-0.452719478359433));
#23987=CARTESIAN_POINT('Ctrl Pts',(1.91718342555755,-1.,-0.449632260106662));
#23988=CARTESIAN_POINT('Ctrl Pts',(1.9120369998112,-1.,-0.446617343485711));
#23989=CARTESIAN_POINT('Ctrl Pts',(1.90691756144898,-1.,-0.443677556849151));
#23990=CARTESIAN_POINT('Ctrl Pts',(1.90180124389086,-1.,-0.440807833704038));
#23991=CARTESIAN_POINT('Ctrl Pts',(1.89663648956466,-1.,-0.437995003948244));
#23992=CARTESIAN_POINT('Ctrl Pts',(1.89136993975504,-1.,-0.435225660963383));
#23993=CARTESIAN_POINT('Ctrl Pts',(1.88596913666793,-1.,-0.432493038548748));
#23994=CARTESIAN_POINT('Ctrl Pts',(1.88044229001832,-1.,-0.429803062482345));
#23995=CARTESIAN_POINT('Ctrl Pts',(1.87486989291484,-1.,-0.427183828519102));
#23996=CARTESIAN_POINT('Ctrl Pts',(1.86937803944323,-1.,-0.424678177291359));
#23997=CARTESIAN_POINT('Ctrl Pts',(1.86408083334028,-1.,-0.422327307418275));
#23998=CARTESIAN_POINT('Ctrl Pts',(1.85903281096686,-1.,-0.42015728797562));
#23999=CARTESIAN_POINT('Ctrl Pts',(1.85417632856234,-1.,-0.418164129143534));
#24000=CARTESIAN_POINT('Ctrl Pts',(1.84929312929882,-1.,-0.416300022038864));
#24001=CARTESIAN_POINT('Ctrl Pts',(1.8440575707371,-1.,-0.41448743825434));
#24002=CARTESIAN_POINT('Ctrl Pts',(1.83808953475839,-1.,-0.412633125322162));
#24003=CARTESIAN_POINT('Ctrl Pts',(1.83100408895216,-1.,-0.410641256301675));
#24004=CARTESIAN_POINT('Ctrl Pts',(1.8224702267854,-1.,-0.408428948108534));
#24005=CARTESIAN_POINT('Ctrl Pts',(1.81223801813988,-1.,-0.405933518411838));
#24006=CARTESIAN_POINT('Ctrl Pts',(1.80012077176221,-1.,-0.403107976170441));
#24007=CARTESIAN_POINT('Ctrl Pts',(1.78598826347533,-1.,-0.399919403783081));
#24008=CARTESIAN_POINT('Ctrl Pts',(1.7697556004756,-1.,-0.39634619612042));
#24009=CARTESIAN_POINT('Ctrl Pts',(1.75137405313962,-1.,-0.392375812294307));
#24010=CARTESIAN_POINT('Ctrl Pts',(1.7349317097561,-1.,-0.388877023509192));
#24011=CARTESIAN_POINT('Ctrl Pts',(1.72162022246158,-1.,-0.38607079032701));
#24012=CARTESIAN_POINT('Ctrl Pts',(1.71231062891958,-1.,-0.384119047315542));
#24013=CARTESIAN_POINT('Ctrl Pts',(1.7075470150345,-1.,-0.383122945602004));
#24014=CARTESIAN_POINT('',(1.74236521665491,-1.,-0.163289472382896));
#24015=CARTESIAN_POINT('Origin',(0.,-1.,0.));
#24016=CARTESIAN_POINT('',(2.19890268624765,-1.,-0.0694764450219582));
#24017=CARTESIAN_POINT('Ctrl Pts',(1.74236521665491,-1.,-0.163289472382896));
#24018=CARTESIAN_POINT('Ctrl Pts',(1.7472034950333,-1.,-0.163814161002002));
#24019=CARTESIAN_POINT('Ctrl Pts',(1.75666056638427,-1.,-0.164834765707159));
#24020=CARTESIAN_POINT('Ctrl Pts',(1.77018771684844,-1.,-0.1662793551464));
#24021=CARTESIAN_POINT('Ctrl Pts',(1.7869064998507,-1.,-0.168032772805197));
#24022=CARTESIAN_POINT('Ctrl Pts',(1.80561530629706,-1.,-0.169936923904608));
#24023=CARTESIAN_POINT('Ctrl Pts',(1.82215766811545,-1.,-0.171554770204119));
#24024=CARTESIAN_POINT('Ctrl Pts',(1.83658380527692,-1.,-0.1728894428919));
#24025=CARTESIAN_POINT('Ctrl Pts',(1.8489811319852,-1.,-0.173946627587732));
#24026=CARTESIAN_POINT('Ctrl Pts',(1.85948367088837,-1.,-0.17473525927603));
#24027=CARTESIAN_POINT('Ctrl Pts',(1.86828349694799,-1.,-0.175268337590758));
#24028=CARTESIAN_POINT('Ctrl Pts',(1.87563767773588,-1.,-0.175563480746485));
#24029=CARTESIAN_POINT('Ctrl Pts',(1.88188663145367,-1.,-0.175644148889699));
#24030=CARTESIAN_POINT('Ctrl Pts',(1.88742606273259,-1.,-0.175538155840648));
#24031=CARTESIAN_POINT('Ctrl Pts',(1.892646301985,-1.,-0.175274276190844));
#24032=CARTESIAN_POINT('Ctrl Pts',(1.89788101117132,-1.,-0.174879405091263));
#24033=CARTESIAN_POINT('Ctrl Pts',(1.90335253862834,-1.,-0.174375518661085));
#24034=CARTESIAN_POINT('Ctrl Pts',(1.90911693975267,-1.,-0.173776635257817));
#24035=CARTESIAN_POINT('Ctrl Pts',(1.91511429159527,-1.,-0.173090695383496));
#24036=CARTESIAN_POINT('Ctrl Pts',(1.9212233439798,-1.,-0.172321621259514));
#24037=CARTESIAN_POINT('Ctrl Pts',(1.92731093582036,-1.,-0.171471191532988));
#24038=CARTESIAN_POINT('Ctrl Pts',(1.93329183155539,-1.,-0.170541253116202));
#24039=CARTESIAN_POINT('Ctrl Pts',(1.93915639211581,-1.,-0.169534904817491));
#24040=CARTESIAN_POINT('Ctrl Pts',(1.94493757756931,-1.,-0.168455741607556));
#24041=CARTESIAN_POINT('Ctrl Pts',(1.95069027794294,-1.,-0.167307501784476));
#24042=CARTESIAN_POINT('Ctrl Pts',(1.9564675971873,-1.,-0.166093592002813));
#24043=CARTESIAN_POINT('Ctrl Pts',(1.96229379940136,-1.,-0.164816568920269));
#24044=CARTESIAN_POINT('Ctrl Pts',(1.96816512677967,-1.,-0.163478185457734));
#24045=CARTESIAN_POINT('Ctrl Pts',(1.97406280235188,-1.,-0.162079693556289));
#24046=CARTESIAN_POINT('Ctrl Pts',(1.97996195437559,-1.,-0.160622060784611));
#24047=CARTESIAN_POINT('Ctrl Pts',(1.98584238283292,-1.,-0.159106226437299));
#24048=CARTESIAN_POINT('Ctrl Pts',(1.99169810931908,-1.,-0.157533331459227));
#24049=CARTESIAN_POINT('Ctrl Pts',(1.99753284771497,-1.,-0.155904629548784));
#24050=CARTESIAN_POINT('Ctrl Pts',(2.00335565310543,-1.,-0.154221403049722));
#24051=CARTESIAN_POINT('Ctrl Pts',(2.00917680318424,-1.,-0.15248488362145));
#24052=CARTESIAN_POINT('Ctrl Pts',(2.01500291940238,-1.,-0.150696157673078));
#24053=CARTESIAN_POINT('Ctrl Pts',(2.02083464969894,-1.,-0.148856124775337));
#24054=CARTESIAN_POINT('Ctrl Pts',(2.02666926182017,-1.,-0.146965557332583));
#24055=CARTESIAN_POINT('Ctrl Pts',(2.03250223739942,-1.,-0.145025140186058));
#24056=CARTESIAN_POINT('Ctrl Pts',(2.03832911025912,-1.,-0.143035515058209));
#24057=CARTESIAN_POINT('Ctrl Pts',(2.04414757947916,-1.,-0.140997332152546));
#24058=CARTESIAN_POINT('Ctrl Pts',(2.04995762001328,-1.,-0.138911255368966));
#24059=CARTESIAN_POINT('Ctrl Pts',(2.05576044414264,-1.,-0.136777941218044));
#24060=CARTESIAN_POINT('Ctrl Pts',(2.06155781517842,-1.,-0.134598026192106));
#24061=CARTESIAN_POINT('Ctrl Pts',(2.06735123910326,-1.,-0.132372111547711));
#24062=CARTESIAN_POINT('Ctrl Pts',(2.07314114713063,-1.,-0.130100748328404));
#24063=CARTESIAN_POINT('Ctrl Pts',(2.07892715110987,-1.,-0.12778444527612));
#24064=CARTESIAN_POINT('Ctrl Pts',(2.08470840653643,-1.,-0.125423679412062));
#24065=CARTESIAN_POINT('Ctrl Pts',(2.09048392424825,-1.,-0.123018905621083));
#24066=CARTESIAN_POINT('Ctrl Pts',(2.0962529286773,-1.,-0.120570567965122));
#24067=CARTESIAN_POINT('Ctrl Pts',(2.102015121329,-1.,-0.118079107988356));
#24068=CARTESIAN_POINT('Ctrl Pts',(2.10777050261309,-1.,-0.115544957687927));
#24069=CARTESIAN_POINT('Ctrl Pts',(2.11351924490306,-1.,-0.112968534419737));
#24070=CARTESIAN_POINT('Ctrl Pts',(2.11926155590865,-1.,-0.110350236135025));
#24071=CARTESIAN_POINT('Ctrl Pts',(2.12499752307,-1.,-0.10769043523109));
#24072=CARTESIAN_POINT('Ctrl Pts',(2.13072704887293,-1.,-0.10498947915274));
#24073=CARTESIAN_POINT('Ctrl Pts',(2.13644992667165,-1.,-0.102247700556101));
#24074=CARTESIAN_POINT('Ctrl Pts',(2.14216588396025,-1.,-0.0994654261990917));
#24075=CARTESIAN_POINT('Ctrl Pts',(2.14787463531795,-1.,-0.096642985230546));
#24076=CARTESIAN_POINT('Ctrl Pts',(2.1535759397817,-1.,-0.0937807218867645));
#24077=CARTESIAN_POINT('Ctrl Pts',(2.15926961544516,-1.,-0.0908789888107267));
#24078=CARTESIAN_POINT('Ctrl Pts',(2.16495552645014,-1.,-0.0879381291386924));
#24079=CARTESIAN_POINT('Ctrl Pts',(2.17063357870952,-1.,-0.0849584620835374));
#24080=CARTESIAN_POINT('Ctrl Pts',(2.176303712113,-1.,-0.0819402680872767));
#24081=CARTESIAN_POINT('Ctrl Pts',(2.18196589448887,-1.,-0.0788837727685244));
#24082=CARTESIAN_POINT('Ctrl Pts',(2.1876201139953,-1.,-0.0757891465836149));
#24083=CARTESIAN_POINT('Ctrl Pts',(2.19213712013662,-1.,-0.0732830357306726));
#24084=CARTESIAN_POINT('Ctrl Pts',(2.19552129484002,-1.,-0.0713863779526155));
#24085=CARTESIAN_POINT('Ctrl Pts',(2.19777582085423,-1.,-0.0701143536325491));
#24086=CARTESIAN_POINT('Ctrl Pts',(2.19890268624765,-1.,-0.0694764450219582));
#24087=CARTESIAN_POINT('',(2.19890268624765,-1.,0.0694764450219582));
#24088=CARTESIAN_POINT('',(2.19890268624765,-1.,-0.0694764450219582));
#24089=CARTESIAN_POINT('',(1.74236521665491,-1.,0.163289472382896));
#24090=CARTESIAN_POINT('Ctrl Pts',(2.19890268624765,-1.,0.0694764450219582));
#24091=CARTESIAN_POINT('Ctrl Pts',(2.19777582085261,-1.,0.0701143536324925));
#24092=CARTESIAN_POINT('Ctrl Pts',(2.19552129483562,-1.,0.0713863779524626));
#24093=CARTESIAN_POINT('Ctrl Pts',(2.19213712012956,-1.,0.0732830357304275));
#24094=CARTESIAN_POINT('Ctrl Pts',(2.1876201139874,-1.,0.075789146583341));
#24095=CARTESIAN_POINT('Ctrl Pts',(2.18196589448304,-1.,0.0788837727683226));
#24096=CARTESIAN_POINT('Ctrl Pts',(2.1763037121106,-1.,0.0819402680871938));
#24097=CARTESIAN_POINT('Ctrl Pts',(2.17063357871031,-1.,0.0849584620835642));
#24098=CARTESIAN_POINT('Ctrl Pts',(2.16495552645275,-1.,0.0879381291387821));
#24099=CARTESIAN_POINT('Ctrl Pts',(2.15926961544808,-1.,0.0908789888108265));
#24100=CARTESIAN_POINT('Ctrl Pts',(2.15357593978377,-1.,0.0937807218868344));
#24101=CARTESIAN_POINT('Ctrl Pts',(2.14787463531864,-1.,0.0966429852305688));
#24102=CARTESIAN_POINT('Ctrl Pts',(2.14216588395974,-1.,0.0994654261990741));
#24103=CARTESIAN_POINT('Ctrl Pts',(2.13644992667052,-1.,0.102247700556063));
#24104=CARTESIAN_POINT('Ctrl Pts',(2.1307270488718,-1.,0.104989479152703));
#24105=CARTESIAN_POINT('Ctrl Pts',(2.12499752306927,-1.,0.107690435231068));
#24106=CARTESIAN_POINT('Ctrl Pts',(2.11926155590849,-1.,0.11035023613502));
#24107=CARTESIAN_POINT('Ctrl Pts',(2.11351924490335,-1.,0.112968534419746));
#24108=CARTESIAN_POINT('Ctrl Pts',(2.10777050261359,-1.,0.11554495768794));
#24109=CARTESIAN_POINT('Ctrl Pts',(2.10201512132945,-1.,0.118079107988368));
#24110=CARTESIAN_POINT('Ctrl Pts',(2.09625292867756,-1.,0.120570567965129));
#24111=CARTESIAN_POINT('Ctrl Pts',(2.09048392424826,-1.,0.123018905621083));
#24112=CARTESIAN_POINT('Ctrl Pts',(2.08470840653628,-1.,0.125423679412058));
#24113=CARTESIAN_POINT('Ctrl Pts',(2.07892715110967,-1.,0.127784445276116));
#24114=CARTESIAN_POINT('Ctrl Pts',(2.07314114713047,-1.,0.1301007483284));
#24115=CARTESIAN_POINT('Ctrl Pts',(2.06735123910319,-1.,0.132372111547709));
#24116=CARTESIAN_POINT('Ctrl Pts',(2.06155781517844,-1.,0.134598026192107));
#24117=CARTESIAN_POINT('Ctrl Pts',(2.0557604441427,-1.,0.136777941218044));
#24118=CARTESIAN_POINT('Ctrl Pts',(2.04995762001333,-1.,0.138911255368966));
#24119=CARTESIAN_POINT('Ctrl Pts',(2.04414757947919,-1.,0.140997332152545));
#24120=CARTESIAN_POINT('Ctrl Pts',(2.03832911025913,-1.,0.143035515058208));
#24121=CARTESIAN_POINT('Ctrl Pts',(2.03250223739941,-1.,0.145025140186058));
#24122=CARTESIAN_POINT('Ctrl Pts',(2.02666926182017,-1.,0.146965557332586));
#24123=CARTESIAN_POINT('Ctrl Pts',(2.02083464969897,-1.,0.148856124775342));
#24124=CARTESIAN_POINT('Ctrl Pts',(2.01500291940243,-1.,0.150696157673084));
#24125=CARTESIAN_POINT('Ctrl Pts',(2.00917680318426,-1.,0.152484883621452));
#24126=CARTESIAN_POINT('Ctrl Pts',(2.00335565310539,-1.,0.154221403049719));
#24127=CARTESIAN_POINT('Ctrl Pts',(1.99753284771487,-1.,0.155904629548774));
#24128=CARTESIAN_POINT('Ctrl Pts',(1.99169810931893,-1.,0.157533331459215));
#24129=CARTESIAN_POINT('Ctrl Pts',(1.98584238283279,-1.,0.159106226437288));
#24130=CARTESIAN_POINT('Ctrl Pts',(1.97996195437557,-1.,0.16062206078461));
#24131=CARTESIAN_POINT('Ctrl Pts',(1.97406280235204,-1.,0.162079693556302));
#24132=CARTESIAN_POINT('Ctrl Pts',(1.96816512678,-1.,0.16347818545776));
#24133=CARTESIAN_POINT('Ctrl Pts',(1.96229379940174,-1.,0.1648165689203));
#24134=CARTESIAN_POINT('Ctrl Pts',(1.95646759718755,-1.,0.166093592002832));
#24135=CARTESIAN_POINT('Ctrl Pts',(1.95069027794286,-1.,0.167307501784469));
#24136=CARTESIAN_POINT('Ctrl Pts',(1.94493757756879,-1.,0.168455741607515));
#24137=CARTESIAN_POINT('Ctrl Pts',(1.93915639211497,-1.,0.169534904817425));
#24138=CARTESIAN_POINT('Ctrl Pts',(1.93329183155455,-1.,0.170541253116136));
#24139=CARTESIAN_POINT('Ctrl Pts',(1.92731093582,-1.,0.17147119153296));
#24140=CARTESIAN_POINT('Ctrl Pts',(1.92122334398034,-1.,0.172321621259556));
#24141=CARTESIAN_POINT('Ctrl Pts',(1.91511429159681,-1.,0.173090695383619));
#24142=CARTESIAN_POINT('Ctrl Pts',(1.90911693975475,-1.,0.173776635257983));
#24143=CARTESIAN_POINT('Ctrl Pts',(1.90335253863003,-1.,0.174375518661222));
#24144=CARTESIAN_POINT('Ctrl Pts',(1.89788101117148,-1.,0.174879405091277));
#24145=CARTESIAN_POINT('Ctrl Pts',(1.89264630198279,-1.,0.175274276190664));
#24146=CARTESIAN_POINT('Ctrl Pts',(1.88742606272818,-1.,0.175538155840286));
#24147=CARTESIAN_POINT('Ctrl Pts',(1.88188663144846,-1.,0.175644148889271));
#24148=CARTESIAN_POINT('Ctrl Pts',(1.87563767773249,-1.,0.175563480746205));
#24149=CARTESIAN_POINT('Ctrl Pts',(1.86828349694972,-1.,0.1752683375909));
#24150=CARTESIAN_POINT('Ctrl Pts',(1.85948367089838,-1.,0.174735259276856));
#24151=CARTESIAN_POINT('Ctrl Pts',(1.84898113200543,-1.,0.173946627589401));
#24152=CARTESIAN_POINT('Ctrl Pts',(1.83658380530747,-1.,0.17288944289442));
#24153=CARTESIAN_POINT('Ctrl Pts',(1.82215766815414,-1.,0.171554770207306));
#24154=CARTESIAN_POINT('Ctrl Pts',(1.80561530633924,-1.,0.169936923908078));
#24155=CARTESIAN_POINT('Ctrl Pts',(1.78690649988931,-1.,0.16803277280837));
#24156=CARTESIAN_POINT('Ctrl Pts',(1.77018771687692,-1.,0.166279355148738));
#24157=CARTESIAN_POINT('Ctrl Pts',(1.75666056640041,-1.,0.164834765708484));
#24158=CARTESIAN_POINT('Ctrl Pts',(1.74720349503904,-1.,0.163814161002474));
#24159=CARTESIAN_POINT('Ctrl Pts',(1.74236521665491,-1.,0.163289472382896));
#24160=CARTESIAN_POINT('',(1.7075470150345,-1.,0.383122945602004));
#24161=CARTESIAN_POINT('Origin',(0.,-1.,0.));
#24162=CARTESIAN_POINT('',(2.11275013067528,-1.,0.613422273260091));
#24163=CARTESIAN_POINT('Ctrl Pts',(1.7075470150345,-1.,0.383122945602004));
#24164=CARTESIAN_POINT('Ctrl Pts',(1.71231062891398,-1.,0.384119047314215));
#24165=CARTESIAN_POINT('Ctrl Pts',(1.72162022244582,-1.,0.386070790323281));
#24166=CARTESIAN_POINT('Ctrl Pts',(1.73493170972829,-1.,0.388877023502615));
#24167=CARTESIAN_POINT('Ctrl Pts',(1.75137405310193,-1.,0.392375812285396));
#24168=CARTESIAN_POINT('Ctrl Pts',(1.76975560043442,-1.,0.396346196110688));
#24169=CARTESIAN_POINT('Ctrl Pts',(1.78598826343754,-1.,0.399919403774156));
#24170=CARTESIAN_POINT('Ctrl Pts',(1.80012077173238,-1.,0.403107976163396));
#24171=CARTESIAN_POINT('Ctrl Pts',(1.81223801812013,-1.,0.405933518407176));
#24172=CARTESIAN_POINT('Ctrl Pts',(1.82247022677562,-1.,0.408428948106228));
#24173=CARTESIAN_POINT('Ctrl Pts',(1.83100408895047,-1.,0.410641256301276));
#24174=CARTESIAN_POINT('Ctrl Pts',(1.8380895347617,-1.,0.412633125322945));
#24175=CARTESIAN_POINT('Ctrl Pts',(1.84405757074218,-1.,0.414487438255542));
#24176=CARTESIAN_POINT('Ctrl Pts',(1.84929312930314,-1.,0.416300022039885));
#24177=CARTESIAN_POINT('Ctrl Pts',(1.8541763285645,-1.,0.418164129144046));
#24178=CARTESIAN_POINT('Ctrl Pts',(1.8590328109667,-1.,0.420157287975583));
#24179=CARTESIAN_POINT('Ctrl Pts',(1.86408083333863,-1.,0.422327307417885));
#24180=CARTESIAN_POINT('Ctrl Pts',(1.8693780394412,-1.,0.424678177290876));
#24181=CARTESIAN_POINT('Ctrl Pts',(1.87486989291333,-1.,0.427183828518743));
#24182=CARTESIAN_POINT('Ctrl Pts',(1.88044229001778,-1.,0.429803062482217));
#24183=CARTESIAN_POINT('Ctrl Pts',(1.88596913666828,-1.,0.432493038548833));
#24184=CARTESIAN_POINT('Ctrl Pts',(1.89136993975585,-1.,0.43522566096358));
#24185=CARTESIAN_POINT('Ctrl Pts',(1.89663648956549,-1.,0.437995003948443));
#24186=CARTESIAN_POINT('Ctrl Pts',(1.90180124389137,-1.,0.440807833704161));
#24187=CARTESIAN_POINT('Ctrl Pts',(1.90691756144906,-1.,0.443677556849171));
#24188=CARTESIAN_POINT('Ctrl Pts',(1.91203699981095,-1.,0.446617343485651));
#24189=CARTESIAN_POINT('Ctrl Pts',(1.91718342555717,-1.,0.449632260106572));
#24190=CARTESIAN_POINT('Ctrl Pts',(1.9223538064847,-1.,0.452719478359356));
#24191=CARTESIAN_POINT('Ctrl Pts',(1.92753067150461,-1.,0.455872005174336));
#24192=CARTESIAN_POINT('Ctrl Pts',(1.93269066517936,-1.,0.459081234547932));
#24193=CARTESIAN_POINT('Ctrl Pts',(1.93781486640834,-1.,0.462340031009087));
#24194=CARTESIAN_POINT('Ctrl Pts',(1.94289794196205,-1.,0.465645462026065));
#24195=CARTESIAN_POINT('Ctrl Pts',(1.94794381136524,-1.,0.468997482913158));
#24196=CARTESIAN_POINT('Ctrl Pts',(1.95296148278136,-1.,0.47239767226408));
#24197=CARTESIAN_POINT('Ctrl Pts',(1.95796111148175,-1.,0.475848034683172));
#24198=CARTESIAN_POINT('Ctrl Pts',(1.96294933055938,-1.,0.479349583074846));
#24199=CARTESIAN_POINT('Ctrl Pts',(1.96792703422358,-1.,0.482901662120687));
#24200=CARTESIAN_POINT('Ctrl Pts',(1.97289186263272,-1.,0.486502692907661));
#24201=CARTESIAN_POINT('Ctrl Pts',(1.97783973019229,-1.,0.490150627860955));
#24202=CARTESIAN_POINT('Ctrl Pts',(1.9827665876182,-1.,0.493843476541493));
#24203=CARTESIAN_POINT('Ctrl Pts',(1.98767044752929,-1.,0.497579909545564));
#24204=CARTESIAN_POINT('Ctrl Pts',(1.9925514912615,-1.,0.501359287727129));
#24205=CARTESIAN_POINT('Ctrl Pts',(1.99741107463567,-1.,0.505181361323011));
#24206=CARTESIAN_POINT('Ctrl Pts',(2.00225107134733,-1.,0.509046069886152));
#24207=CARTESIAN_POINT('Ctrl Pts',(2.00707309946955,-1.,0.512953306961814));
#24208=CARTESIAN_POINT('Ctrl Pts',(2.01187773939257,-1.,0.516902681728733));
#24209=CARTESIAN_POINT('Ctrl Pts',(2.01666477917305,-1.,0.520893590399429));
#24210=CARTESIAN_POINT('Ctrl Pts',(2.02143356304712,-1.,0.524925318333519));
#24211=CARTESIAN_POINT('Ctrl Pts',(2.02618329083289,-1.,0.528997127241911));
#24212=CARTESIAN_POINT('Ctrl Pts',(2.03091336214401,-1.,0.533108355132905));
#24213=CARTESIAN_POINT('Ctrl Pts',(2.03562362953993,-1.,0.537258489833135));
#24214=CARTESIAN_POINT('Ctrl Pts',(2.0403142269048,-1.,0.54144712061552));
#24215=CARTESIAN_POINT('Ctrl Pts',(2.0449854471456,-1.,0.545673903817349));
#24216=CARTESIAN_POINT('Ctrl Pts',(2.04963761077974,-1.,0.549938525150342));
#24217=CARTESIAN_POINT('Ctrl Pts',(2.05427091604482,-1.,0.55424065746411));
#24218=CARTESIAN_POINT('Ctrl Pts',(2.05888537756571,-1.,0.558579940185468));
#24219=CARTESIAN_POINT('Ctrl Pts',(2.06348090160697,-1.,0.562955993082574));
#24220=CARTESIAN_POINT('Ctrl Pts',(2.06805732997383,-1.,0.56736842118123));
#24221=CARTESIAN_POINT('Ctrl Pts',(2.07261449292757,-1.,0.571816823242411));
#24222=CARTESIAN_POINT('Ctrl Pts',(2.07715226767361,-1.,0.576300797416275));
#24223=CARTESIAN_POINT('Ctrl Pts',(2.08167059018138,-1.,0.580819952107257));
#24224=CARTESIAN_POINT('Ctrl Pts',(2.086169437277,-1.,0.585373918990895));
#24225=CARTESIAN_POINT('Ctrl Pts',(2.09064881812053,-1.,0.58996236540319));
#24226=CARTESIAN_POINT('Ctrl Pts',(2.09510876220501,-1.,0.594585006052824));
#24227=CARTESIAN_POINT('Ctrl Pts',(2.09954930865331,-1.,0.599241616422144));
#24228=CARTESIAN_POINT('Ctrl Pts',(2.10397049887709,-1.,0.603932030738212));
#24229=CARTESIAN_POINT('Ctrl Pts',(2.10749199615859,-1.,0.607711315456826));
#24230=CARTESIAN_POINT('Ctrl Pts',(2.11012443807661,-1.,0.610560911691114));
#24231=CARTESIAN_POINT('Ctrl Pts',(2.11187554260142,-1.,0.61246736556225));
#24232=CARTESIAN_POINT('Ctrl Pts',(2.11275013067528,-1.,0.613422273260091));
#24233=CARTESIAN_POINT('',(2.0698113262342,-1.,0.745574324794401));
#24234=CARTESIAN_POINT('',(2.11275013067528,-1.,0.613422273260091));
#24235=CARTESIAN_POINT('Ctrl Pts',(2.0698113262342,-1.,0.745574324794401));
#24236=CARTESIAN_POINT('Ctrl Pts',(2.06854248895575,-1.,0.74583279137781));
#24237=CARTESIAN_POINT('Ctrl Pts',(2.06600523016401,-1.,0.746345871542696));
#24238=CARTESIAN_POINT('Ctrl Pts',(2.06220058927162,-1.,0.747103932785504));
#24239=CARTESIAN_POINT('Ctrl Pts',(2.05713023030263,-1.,0.748091554181101));
#24240=CARTESIAN_POINT('Ctrl Pts',(2.05079645591606,-1.,0.749287468663053));
#24241=CARTESIAN_POINT('Ctrl Pts',(2.04446689147754,-1.,0.750444657874758));
#24242=CARTESIAN_POINT('Ctrl Pts',(2.03814160092173,-1.,0.751562963361384));
#24243=CARTESIAN_POINT('Ctrl Pts',(2.03182068456467,-1.,0.752642180488104));
#24244=CARTESIAN_POINT('Ctrl Pts',(2.02550428623587,-1.,0.753682061113766));
#24245=CARTESIAN_POINT('Ctrl Pts',(2.01919259406003,-1.,0.75468233072352));
#24246=CARTESIAN_POINT('Ctrl Pts',(2.01288584328149,-1.,0.755642704958101));
#24247=CARTESIAN_POINT('Ctrl Pts',(2.00658431587682,-1.,0.756562904646496));
#24248=CARTESIAN_POINT('Ctrl Pts',(2.00028834739072,-1.,0.757442676862342));
#24249=CARTESIAN_POINT('Ctrl Pts',(1.9939983109871,-1.,0.758281796766377));
#24250=CARTESIAN_POINT('Ctrl Pts',(1.98771456680806,-1.,0.759080037802243));
#24251=CARTESIAN_POINT('Ctrl Pts',(1.98143741418156,-1.,0.759837147452135));
#24252=CARTESIAN_POINT('Ctrl Pts',(1.97516705321521,-1.,0.760552825409856));
#24253=CARTESIAN_POINT('Ctrl Pts',(1.96890351582545,-1.,0.761226690483986));
#24254=CARTESIAN_POINT('Ctrl Pts',(1.96264672744229,-1.,0.761858300014575));
#24255=CARTESIAN_POINT('Ctrl Pts',(1.95639665309893,-1.,0.762447203806264));
#24256=CARTESIAN_POINT('Ctrl Pts',(1.95015342590025,-1.,0.762992990878774));
#24257=CARTESIAN_POINT('Ctrl Pts',(1.94391746617626,-1.,0.763495333538581));
#24258=CARTESIAN_POINT('Ctrl Pts',(1.93768964875867,-1.,0.763954049121394));
#24259=CARTESIAN_POINT('Ctrl Pts',(1.93147105496367,-1.,0.76436901067389));
#24260=CARTESIAN_POINT('Ctrl Pts',(1.92526263537041,-1.,0.764740025488189));
#24261=CARTESIAN_POINT('Ctrl Pts',(1.91906491634197,-1.,0.765066729667095));
#24262=CARTESIAN_POINT('Ctrl Pts',(1.91287765805174,-1.,0.765348465884739));
#24263=CARTESIAN_POINT('Ctrl Pts',(1.90669961402362,-1.,0.765584196937937));
#24264=CARTESIAN_POINT('Ctrl Pts',(1.90052930393599,-1.,0.765772772593395));
#24265=CARTESIAN_POINT('Ctrl Pts',(1.89436577771389,-1.,0.765913193856979));
#24266=CARTESIAN_POINT('Ctrl Pts',(1.88820926433409,-1.,0.76600483706209));
#24267=CARTESIAN_POINT('Ctrl Pts',(1.88206215302561,-1.,0.766047794851869));
#24268=CARTESIAN_POINT('Ctrl Pts',(1.87592888967886,-1.,0.766042837036759));
#24269=CARTESIAN_POINT('Ctrl Pts',(1.86981398314345,-1.,0.765990708546112));
#24270=CARTESIAN_POINT('Ctrl Pts',(1.86372027063314,-1.,0.765891519092557));
#24271=CARTESIAN_POINT('Ctrl Pts',(1.85764741390391,-1.,0.765744212909305));
#24272=CARTESIAN_POINT('Ctrl Pts',(1.85158945130054,-1.,0.765545710619023));
#24273=CARTESIAN_POINT('Ctrl Pts',(1.8455369887591,-1.,0.765291664861972));
#24274=CARTESIAN_POINT('Ctrl Pts',(1.83948181064823,-1.,0.764978057881688));
#24275=CARTESIAN_POINT('Ctrl Pts',(1.8334207722714,-1.,0.764602549687846));
#24276=CARTESIAN_POINT('Ctrl Pts',(1.8273599120008,-1.,0.764165902606056));
#24277=CARTESIAN_POINT('Ctrl Pts',(1.82131873145297,-1.,0.763673465462854));
#24278=CARTESIAN_POINT('Ctrl Pts',(1.81532118405566,-1.,0.763132003836783));
#24279=CARTESIAN_POINT('Ctrl Pts',(1.80938551463989,-1.,0.762546129464036));
#24280=CARTESIAN_POINT('Ctrl Pts',(1.80351583877334,-1.,0.761915336443516));
#24281=CARTESIAN_POINT('Ctrl Pts',(1.79768986997735,-1.,0.761229695230359));
#24282=CARTESIAN_POINT('Ctrl Pts',(1.79185815610802,-1.,0.760469555880425));
#24283=CARTESIAN_POINT('Ctrl Pts',(1.78596964884526,-1.,0.759614401109868));
#24284=CARTESIAN_POINT('Ctrl Pts',(1.77999411220912,-1.,0.75865062667738));
#24285=CARTESIAN_POINT('Ctrl Pts',(1.77394167108342,-1.,0.757578264077238));
#24286=CARTESIAN_POINT('Ctrl Pts',(1.76789396003141,-1.,0.756421896028403));
#24287=CARTESIAN_POINT('Ctrl Pts',(1.7619781724032,-1.,0.755220979975262));
#24288=CARTESIAN_POINT('Ctrl Pts',(1.75631083600175,-1.,0.75400925402848));
#24289=CARTESIAN_POINT('Ctrl Pts',(1.75095139468809,-1.,0.752797683531377));
#24290=CARTESIAN_POINT('Ctrl Pts',(1.74585086852298,-1.,0.751555614163629));
#24291=CARTESIAN_POINT('Ctrl Pts',(1.74080458266705,-1.,0.750193435979541));
#24292=CARTESIAN_POINT('Ctrl Pts',(1.73550351679848,-1.,0.748582462954855));
#24293=CARTESIAN_POINT('Ctrl Pts',(1.72958533647399,-1.,0.746574710096437));
#24294=CARTESIAN_POINT('Ctrl Pts',(1.7226822991693,-1.,0.744021445433765));
#24295=CARTESIAN_POINT('Ctrl Pts',(1.71447789751927,-1.,0.740795162032088));
#24296=CARTESIAN_POINT('Ctrl Pts',(1.70473309006121,-1.,0.736799665724771));
#24297=CARTESIAN_POINT('Ctrl Pts',(1.69326921975743,-1.,0.731963238697195));
#24298=CARTESIAN_POINT('Ctrl Pts',(1.67996158455503,-1.,0.726235967997433));
#24299=CARTESIAN_POINT('Ctrl Pts',(1.6647288055568,-1.,0.719585433804282));
#24300=CARTESIAN_POINT('Ctrl Pts',(1.64752408832016,-1.,0.711993139355394));
#24301=CARTESIAN_POINT('Ctrl Pts',(1.63216541664676,-1.,0.705159151988319));
#24302=CARTESIAN_POINT('Ctrl Pts',(1.61974673472612,-1.,0.699605146405088));
#24303=CARTESIAN_POINT('Ctrl Pts',(1.61106790958151,-1.,0.695712097881194));
#24304=CARTESIAN_POINT('Ctrl Pts',(1.60662857109684,-1.,0.693717979106306));
#24305=CARTESIAN_POINT('Origin',(0.,-1.,0.));
#24306=CARTESIAN_POINT('Origin',(0.,0.,0.));
#24307=CARTESIAN_POINT('Origin',(0.,2.2,0.));
#24308=CARTESIAN_POINT('Origin',(0.,1.,0.));
#24309=CARTESIAN_POINT('',(-1.4,2.2,1.71450551880629E-16));
#24310=CARTESIAN_POINT('Origin',(0.,2.2,0.));
#24311=CARTESIAN_POINT('',(-1.4,1.,1.71450551880629E-16));
#24312=CARTESIAN_POINT('',(-1.4,1.,1.71450551880629E-16));
#24313=CARTESIAN_POINT('Origin',(0.,1.,0.));
#24314=CARTESIAN_POINT('Origin',(0.,2.2,0.));
#24315=CARTESIAN_POINT('Ctrl Pts',(2.11275013067528,-1.,0.613422273260091));
#24316=CARTESIAN_POINT('Ctrl Pts',(2.11275013067528,1.,0.613422273260091));
#24317=CARTESIAN_POINT('Ctrl Pts',(2.11187554260142,-1.,0.61246736556225));
#24318=CARTESIAN_POINT('Ctrl Pts',(2.11187554260142,1.,0.61246736556225));
#24319=CARTESIAN_POINT('Ctrl Pts',(2.11012443807661,-1.,0.610560911691114));
#24320=CARTESIAN_POINT('Ctrl Pts',(2.11012443807661,1.,0.610560911691114));
#24321=CARTESIAN_POINT('Ctrl Pts',(2.10749199615859,-1.,0.607711315456826));
#24322=CARTESIAN_POINT('Ctrl Pts',(2.10749199615859,1.,0.607711315456826));
#24323=CARTESIAN_POINT('Ctrl Pts',(2.10397049887709,-1.,0.603932030738212));
#24324=CARTESIAN_POINT('Ctrl Pts',(2.10397049887709,1.,0.603932030738212));
#24325=CARTESIAN_POINT('Ctrl Pts',(2.09954930865331,-1.,0.599241616422144));
#24326=CARTESIAN_POINT('Ctrl Pts',(2.09954930865331,1.,0.599241616422144));
#24327=CARTESIAN_POINT('Ctrl Pts',(2.09510876220501,-1.,0.594585006052824));
#24328=CARTESIAN_POINT('Ctrl Pts',(2.09510876220501,1.,0.594585006052824));
#24329=CARTESIAN_POINT('Ctrl Pts',(2.09064881812053,-1.,0.58996236540319));
#24330=CARTESIAN_POINT('Ctrl Pts',(2.09064881812053,1.,0.58996236540319));
#24331=CARTESIAN_POINT('Ctrl Pts',(2.086169437277,-1.,0.585373918990895));
#24332=CARTESIAN_POINT('Ctrl Pts',(2.086169437277,1.,0.585373918990895));
#24333=CARTESIAN_POINT('Ctrl Pts',(2.08167059018138,-1.,0.580819952107257));
#24334=CARTESIAN_POINT('Ctrl Pts',(2.08167059018138,1.,0.580819952107257));
#24335=CARTESIAN_POINT('Ctrl Pts',(2.07715226767361,-1.,0.576300797416275));
#24336=CARTESIAN_POINT('Ctrl Pts',(2.07715226767361,1.,0.576300797416275));
#24337=CARTESIAN_POINT('Ctrl Pts',(2.07261449292757,-1.,0.571816823242411));
#24338=CARTESIAN_POINT('Ctrl Pts',(2.07261449292757,1.,0.571816823242411));
#24339=CARTESIAN_POINT('Ctrl Pts',(2.06805732997383,-1.,0.56736842118123));
#24340=CARTESIAN_POINT('Ctrl Pts',(2.06805732997383,1.,0.56736842118123));
#24341=CARTESIAN_POINT('Ctrl Pts',(2.06348090160697,-1.,0.562955993082574));
#24342=CARTESIAN_POINT('Ctrl Pts',(2.06348090160697,1.,0.562955993082574));
#24343=CARTESIAN_POINT('Ctrl Pts',(2.05888537756571,-1.,0.558579940185468));
#24344=CARTESIAN_POINT('Ctrl Pts',(2.05888537756571,1.,0.558579940185468));
#24345=CARTESIAN_POINT('Ctrl Pts',(2.05427091604482,-1.,0.55424065746411));
#24346=CARTESIAN_POINT('Ctrl Pts',(2.05427091604482,1.,0.55424065746411));
#24347=CARTESIAN_POINT('Ctrl Pts',(2.04963761077974,-1.,0.549938525150342));
#24348=CARTESIAN_POINT('Ctrl Pts',(2.04963761077974,1.,0.549938525150342));
#24349=CARTESIAN_POINT('Ctrl Pts',(2.0449854471456,-1.,0.545673903817349));
#24350=CARTESIAN_POINT('Ctrl Pts',(2.0449854471456,1.,0.545673903817349));
#24351=CARTESIAN_POINT('Ctrl Pts',(2.0403142269048,-1.,0.54144712061552));
#24352=CARTESIAN_POINT('Ctrl Pts',(2.0403142269048,1.,0.54144712061552));
#24353=CARTESIAN_POINT('Ctrl Pts',(2.03562362953993,-1.,0.537258489833135));
#24354=CARTESIAN_POINT('Ctrl Pts',(2.03562362953993,1.,0.537258489833135));
#24355=CARTESIAN_POINT('Ctrl Pts',(2.03091336214401,-1.,0.533108355132905));
#24356=CARTESIAN_POINT('Ctrl Pts',(2.03091336214401,1.,0.533108355132905));
#24357=CARTESIAN_POINT('Ctrl Pts',(2.02618329083289,-1.,0.528997127241911));
#24358=CARTESIAN_POINT('Ctrl Pts',(2.02618329083289,1.,0.528997127241911));
#24359=CARTESIAN_POINT('Ctrl Pts',(2.02143356304712,-1.,0.524925318333519));
#24360=CARTESIAN_POINT('Ctrl Pts',(2.02143356304712,1.,0.524925318333519));
#24361=CARTESIAN_POINT('Ctrl Pts',(2.01666477917305,-1.,0.520893590399429));
#24362=CARTESIAN_POINT('Ctrl Pts',(2.01666477917305,1.,0.520893590399429));
#24363=CARTESIAN_POINT('Ctrl Pts',(2.01187773939257,-1.,0.516902681728733));
#24364=CARTESIAN_POINT('Ctrl Pts',(2.01187773939257,1.,0.516902681728733));
#24365=CARTESIAN_POINT('Ctrl Pts',(2.00707309946955,-1.,0.512953306961814));
#24366=CARTESIAN_POINT('Ctrl Pts',(2.00707309946955,1.,0.512953306961814));
#24367=CARTESIAN_POINT('Ctrl Pts',(2.00225107134733,-1.,0.509046069886152));
#24368=CARTESIAN_POINT('Ctrl Pts',(2.00225107134733,1.,0.509046069886152));
#24369=CARTESIAN_POINT('Ctrl Pts',(1.99741107463567,-1.,0.505181361323011));
#24370=CARTESIAN_POINT('Ctrl Pts',(1.99741107463567,1.,0.505181361323011));
#24371=CARTESIAN_POINT('Ctrl Pts',(1.9925514912615,-1.,0.501359287727129));
#24372=CARTESIAN_POINT('Ctrl Pts',(1.9925514912615,1.,0.501359287727129));
#24373=CARTESIAN_POINT('Ctrl Pts',(1.98767044752929,-1.,0.497579909545564));
#24374=CARTESIAN_POINT('Ctrl Pts',(1.98767044752929,1.,0.497579909545564));
#24375=CARTESIAN_POINT('Ctrl Pts',(1.9827665876182,-1.,0.493843476541493));
#24376=CARTESIAN_POINT('Ctrl Pts',(1.9827665876182,1.,0.493843476541493));
#24377=CARTESIAN_POINT('Ctrl Pts',(1.97783973019229,-1.,0.490150627860955));
#24378=CARTESIAN_POINT('Ctrl Pts',(1.97783973019229,1.,0.490150627860955));
#24379=CARTESIAN_POINT('Ctrl Pts',(1.97289186263272,-1.,0.486502692907661));
#24380=CARTESIAN_POINT('Ctrl Pts',(1.97289186263272,1.,0.486502692907661));
#24381=CARTESIAN_POINT('Ctrl Pts',(1.96792703422358,-1.,0.482901662120687));
#24382=CARTESIAN_POINT('Ctrl Pts',(1.96792703422358,1.,0.482901662120687));
#24383=CARTESIAN_POINT('Ctrl Pts',(1.96294933055938,-1.,0.479349583074846));
#24384=CARTESIAN_POINT('Ctrl Pts',(1.96294933055938,1.,0.479349583074846));
#24385=CARTESIAN_POINT('Ctrl Pts',(1.95796111148175,-1.,0.475848034683172));
#24386=CARTESIAN_POINT('Ctrl Pts',(1.95796111148175,1.,0.475848034683172));
#24387=CARTESIAN_POINT('Ctrl Pts',(1.95296148278136,-1.,0.47239767226408));
#24388=CARTESIAN_POINT('Ctrl Pts',(1.95296148278136,1.,0.47239767226408));
#24389=CARTESIAN_POINT('Ctrl Pts',(1.94794381136524,-1.,0.468997482913158));
#24390=CARTESIAN_POINT('Ctrl Pts',(1.94794381136524,1.,0.468997482913158));
#24391=CARTESIAN_POINT('Ctrl Pts',(1.94289794196205,-1.,0.465645462026065));
#24392=CARTESIAN_POINT('Ctrl Pts',(1.94289794196205,1.,0.465645462026065));
#24393=CARTESIAN_POINT('Ctrl Pts',(1.93781486640834,-1.,0.462340031009087));
#24394=CARTESIAN_POINT('Ctrl Pts',(1.93781486640834,1.,0.462340031009087));
#24395=CARTESIAN_POINT('Ctrl Pts',(1.93269066517936,-1.,0.459081234547932));
#24396=CARTESIAN_POINT('Ctrl Pts',(1.93269066517936,1.,0.459081234547932));
#24397=CARTESIAN_POINT('Ctrl Pts',(1.92753067150461,-1.,0.455872005174336));
#24398=CARTESIAN_POINT('Ctrl Pts',(1.92753067150461,1.,0.455872005174336));
#24399=CARTESIAN_POINT('Ctrl Pts',(1.9223538064847,-1.,0.452719478359356));
#24400=CARTESIAN_POINT('Ctrl Pts',(1.9223538064847,1.,0.452719478359356));
#24401=CARTESIAN_POINT('Ctrl Pts',(1.91718342555717,-1.,0.449632260106572));
#24402=CARTESIAN_POINT('Ctrl Pts',(1.91718342555717,1.,0.449632260106572));
#24403=CARTESIAN_POINT('Ctrl Pts',(1.91203699981095,-1.,0.446617343485651));
#24404=CARTESIAN_POINT('Ctrl Pts',(1.91203699981095,1.,0.446617343485651));
#24405=CARTESIAN_POINT('Ctrl Pts',(1.90691756144906,-1.,0.443677556849171));
#24406=CARTESIAN_POINT('Ctrl Pts',(1.90691756144906,1.,0.443677556849171));
#24407=CARTESIAN_POINT('Ctrl Pts',(1.90180124389137,-1.,0.440807833704161));
#24408=CARTESIAN_POINT('Ctrl Pts',(1.90180124389137,1.,0.440807833704161));
#24409=CARTESIAN_POINT('Ctrl Pts',(1.89663648956549,-1.,0.437995003948443));
#24410=CARTESIAN_POINT('Ctrl Pts',(1.89663648956549,1.,0.437995003948443));
#24411=CARTESIAN_POINT('Ctrl Pts',(1.89136993975585,-1.,0.43522566096358));
#24412=CARTESIAN_POINT('Ctrl Pts',(1.89136993975585,1.,0.43522566096358));
#24413=CARTESIAN_POINT('Ctrl Pts',(1.88596913666828,-1.,0.432493038548833));
#24414=CARTESIAN_POINT('Ctrl Pts',(1.88596913666828,1.,0.432493038548833));
#24415=CARTESIAN_POINT('Ctrl Pts',(1.88044229001778,-1.,0.429803062482217));
#24416=CARTESIAN_POINT('Ctrl Pts',(1.88044229001778,1.,0.429803062482217));
#24417=CARTESIAN_POINT('Ctrl Pts',(1.87486989291333,-1.,0.427183828518743));
#24418=CARTESIAN_POINT('Ctrl Pts',(1.87486989291333,1.,0.427183828518743));
#24419=CARTESIAN_POINT('Ctrl Pts',(1.8693780394412,-1.,0.424678177290876));
#24420=CARTESIAN_POINT('Ctrl Pts',(1.8693780394412,1.,0.424678177290876));
#24421=CARTESIAN_POINT('Ctrl Pts',(1.86408083333863,-1.,0.422327307417885));
#24422=CARTESIAN_POINT('Ctrl Pts',(1.86408083333863,1.,0.422327307417885));
#24423=CARTESIAN_POINT('Ctrl Pts',(1.8590328109667,-1.,0.420157287975583));
#24424=CARTESIAN_POINT('Ctrl Pts',(1.8590328109667,1.,0.420157287975583));
#24425=CARTESIAN_POINT('Ctrl Pts',(1.8541763285645,-1.,0.418164129144046));
#24426=CARTESIAN_POINT('Ctrl Pts',(1.8541763285645,1.,0.418164129144046));
#24427=CARTESIAN_POINT('Ctrl Pts',(1.84929312930314,-1.,0.416300022039885));
#24428=CARTESIAN_POINT('Ctrl Pts',(1.84929312930314,1.,0.416300022039885));
#24429=CARTESIAN_POINT('Ctrl Pts',(1.84405757074218,-1.,0.414487438255542));
#24430=CARTESIAN_POINT('Ctrl Pts',(1.84405757074218,1.,0.414487438255542));
#24431=CARTESIAN_POINT('Ctrl Pts',(1.8380895347617,-1.,0.412633125322945));
#24432=CARTESIAN_POINT('Ctrl Pts',(1.8380895347617,1.,0.412633125322945));
#24433=CARTESIAN_POINT('Ctrl Pts',(1.83100408895047,-1.,0.410641256301276));
#24434=CARTESIAN_POINT('Ctrl Pts',(1.83100408895047,1.,0.410641256301276));
#24435=CARTESIAN_POINT('Ctrl Pts',(1.82247022677562,-1.,0.408428948106228));
#24436=CARTESIAN_POINT('Ctrl Pts',(1.82247022677562,1.,0.408428948106228));
#24437=CARTESIAN_POINT('Ctrl Pts',(1.81223801812013,-1.,0.405933518407176));
#24438=CARTESIAN_POINT('Ctrl Pts',(1.81223801812013,1.,0.405933518407176));
#24439=CARTESIAN_POINT('Ctrl Pts',(1.80012077173238,-1.,0.403107976163396));
#24440=CARTESIAN_POINT('Ctrl Pts',(1.80012077173238,1.,0.403107976163396));
#24441=CARTESIAN_POINT('Ctrl Pts',(1.78598826343754,-1.,0.399919403774156));
#24442=CARTESIAN_POINT('Ctrl Pts',(1.78598826343754,1.,0.399919403774156));
#24443=CARTESIAN_POINT('Ctrl Pts',(1.76975560043442,-1.,0.396346196110688));
#24444=CARTESIAN_POINT('Ctrl Pts',(1.76975560043442,1.,0.396346196110688));
#24445=CARTESIAN_POINT('Ctrl Pts',(1.75137405310193,-1.,0.392375812285396));
#24446=CARTESIAN_POINT('Ctrl Pts',(1.75137405310193,1.,0.392375812285396));
#24447=CARTESIAN_POINT('Ctrl Pts',(1.73493170972829,-1.,0.388877023502615));
#24448=CARTESIAN_POINT('Ctrl Pts',(1.73493170972829,1.,0.388877023502615));
#24449=CARTESIAN_POINT('Ctrl Pts',(1.72162022244582,-1.,0.386070790323281));
#24450=CARTESIAN_POINT('Ctrl Pts',(1.72162022244582,1.,0.386070790323281));
#24451=CARTESIAN_POINT('Ctrl Pts',(1.71231062891398,-1.,0.384119047314215));
#24452=CARTESIAN_POINT('Ctrl Pts',(1.71231062891398,1.,0.384119047314215));
#24453=CARTESIAN_POINT('Ctrl Pts',(1.7075470150345,-1.,0.383122945602004));
#24454=CARTESIAN_POINT('Ctrl Pts',(1.7075470150345,1.,0.383122945602004));
#24455=CARTESIAN_POINT('',(1.7075470150345,1.,0.383122945602004));
#24456=CARTESIAN_POINT('',(1.7075470150345,0.,0.383122945602005));
#24457=CARTESIAN_POINT('',(2.11275013067528,1.,0.613422273260091));
#24458=CARTESIAN_POINT('Ctrl Pts',(2.11275013067528,1.,0.613422273260091));
#24459=CARTESIAN_POINT('Ctrl Pts',(2.11187554260142,1.,0.61246736556225));
#24460=CARTESIAN_POINT('Ctrl Pts',(2.11012443807661,1.,0.610560911691114));
#24461=CARTESIAN_POINT('Ctrl Pts',(2.10749199615859,1.,0.607711315456826));
#24462=CARTESIAN_POINT('Ctrl Pts',(2.10397049887709,1.,0.603932030738212));
#24463=CARTESIAN_POINT('Ctrl Pts',(2.09954930865331,1.,0.599241616422144));
#24464=CARTESIAN_POINT('Ctrl Pts',(2.09510876220501,1.,0.594585006052824));
#24465=CARTESIAN_POINT('Ctrl Pts',(2.09064881812053,1.,0.58996236540319));
#24466=CARTESIAN_POINT('Ctrl Pts',(2.086169437277,1.,0.585373918990895));
#24467=CARTESIAN_POINT('Ctrl Pts',(2.08167059018138,1.,0.580819952107257));
#24468=CARTESIAN_POINT('Ctrl Pts',(2.07715226767361,1.,0.576300797416275));
#24469=CARTESIAN_POINT('Ctrl Pts',(2.07261449292757,1.,0.571816823242411));
#24470=CARTESIAN_POINT('Ctrl Pts',(2.06805732997383,1.,0.56736842118123));
#24471=CARTESIAN_POINT('Ctrl Pts',(2.06348090160697,1.,0.562955993082574));
#24472=CARTESIAN_POINT('Ctrl Pts',(2.05888537756571,1.,0.558579940185468));
#24473=CARTESIAN_POINT('Ctrl Pts',(2.05427091604482,1.,0.55424065746411));
#24474=CARTESIAN_POINT('Ctrl Pts',(2.04963761077974,1.,0.549938525150342));
#24475=CARTESIAN_POINT('Ctrl Pts',(2.0449854471456,1.,0.545673903817349));
#24476=CARTESIAN_POINT('Ctrl Pts',(2.0403142269048,1.,0.54144712061552));
#24477=CARTESIAN_POINT('Ctrl Pts',(2.03562362953993,1.,0.537258489833135));
#24478=CARTESIAN_POINT('Ctrl Pts',(2.03091336214401,1.,0.533108355132905));
#24479=CARTESIAN_POINT('Ctrl Pts',(2.02618329083289,1.,0.528997127241911));
#24480=CARTESIAN_POINT('Ctrl Pts',(2.02143356304712,1.,0.524925318333519));
#24481=CARTESIAN_POINT('Ctrl Pts',(2.01666477917305,1.,0.520893590399429));
#24482=CARTESIAN_POINT('Ctrl Pts',(2.01187773939257,1.,0.516902681728733));
#24483=CARTESIAN_POINT('Ctrl Pts',(2.00707309946955,1.,0.512953306961814));
#24484=CARTESIAN_POINT('Ctrl Pts',(2.00225107134733,1.,0.509046069886152));
#24485=CARTESIAN_POINT('Ctrl Pts',(1.99741107463567,1.,0.505181361323011));
#24486=CARTESIAN_POINT('Ctrl Pts',(1.9925514912615,1.,0.501359287727129));
#24487=CARTESIAN_POINT('Ctrl Pts',(1.98767044752929,1.,0.497579909545564));
#24488=CARTESIAN_POINT('Ctrl Pts',(1.9827665876182,1.,0.493843476541493));
#24489=CARTESIAN_POINT('Ctrl Pts',(1.97783973019229,1.,0.490150627860955));
#24490=CARTESIAN_POINT('Ctrl Pts',(1.97289186263272,1.,0.486502692907661));
#24491=CARTESIAN_POINT('Ctrl Pts',(1.96792703422358,1.,0.482901662120687));
#24492=CARTESIAN_POINT('Ctrl Pts',(1.96294933055938,1.,0.479349583074846));
#24493=CARTESIAN_POINT('Ctrl Pts',(1.95796111148175,1.,0.475848034683172));
#24494=CARTESIAN_POINT('Ctrl Pts',(1.95296148278136,1.,0.47239767226408));
#24495=CARTESIAN_POINT('Ctrl Pts',(1.94794381136524,1.,0.468997482913158));
#24496=CARTESIAN_POINT('Ctrl Pts',(1.94289794196205,1.,0.465645462026065));
#24497=CARTESIAN_POINT('Ctrl Pts',(1.93781486640834,1.,0.462340031009087));
#24498=CARTESIAN_POINT('Ctrl Pts',(1.93269066517936,1.,0.459081234547932));
#24499=CARTESIAN_POINT('Ctrl Pts',(1.92753067150461,1.,0.455872005174336));
#24500=CARTESIAN_POINT('Ctrl Pts',(1.9223538064847,1.,0.452719478359356));
#24501=CARTESIAN_POINT('Ctrl Pts',(1.91718342555717,1.,0.449632260106572));
#24502=CARTESIAN_POINT('Ctrl Pts',(1.91203699981095,1.,0.446617343485651));
#24503=CARTESIAN_POINT('Ctrl Pts',(1.90691756144906,1.,0.443677556849171));
#24504=CARTESIAN_POINT('Ctrl Pts',(1.90180124389137,1.,0.440807833704161));
#24505=CARTESIAN_POINT('Ctrl Pts',(1.89663648956549,1.,0.437995003948443));
#24506=CARTESIAN_POINT('Ctrl Pts',(1.89136993975585,1.,0.43522566096358));
#24507=CARTESIAN_POINT('Ctrl Pts',(1.88596913666828,1.,0.432493038548833));
#24508=CARTESIAN_POINT('Ctrl Pts',(1.88044229001778,1.,0.429803062482217));
#24509=CARTESIAN_POINT('Ctrl Pts',(1.87486989291333,1.,0.427183828518743));
#24510=CARTESIAN_POINT('Ctrl Pts',(1.8693780394412,1.,0.424678177290876));
#24511=CARTESIAN_POINT('Ctrl Pts',(1.86408083333863,1.,0.422327307417885));
#24512=CARTESIAN_POINT('Ctrl Pts',(1.8590328109667,1.,0.420157287975583));
#24513=CARTESIAN_POINT('Ctrl Pts',(1.8541763285645,1.,0.418164129144046));
#24514=CARTESIAN_POINT('Ctrl Pts',(1.84929312930314,1.,0.416300022039885));
#24515=CARTESIAN_POINT('Ctrl Pts',(1.84405757074218,1.,0.414487438255542));
#24516=CARTESIAN_POINT('Ctrl Pts',(1.8380895347617,1.,0.412633125322945));
#24517=CARTESIAN_POINT('Ctrl Pts',(1.83100408895047,1.,0.410641256301276));
#24518=CARTESIAN_POINT('Ctrl Pts',(1.82247022677562,1.,0.408428948106228));
#24519=CARTESIAN_POINT('Ctrl Pts',(1.81223801812013,1.,0.405933518407176));
#24520=CARTESIAN_POINT('Ctrl Pts',(1.80012077173238,1.,0.403107976163396));
#24521=CARTESIAN_POINT('Ctrl Pts',(1.78598826343754,1.,0.399919403774156));
#24522=CARTESIAN_POINT('Ctrl Pts',(1.76975560043442,1.,0.396346196110688));
#24523=CARTESIAN_POINT('Ctrl Pts',(1.75137405310193,1.,0.392375812285396));
#24524=CARTESIAN_POINT('Ctrl Pts',(1.73493170972829,1.,0.388877023502615));
#24525=CARTESIAN_POINT('Ctrl Pts',(1.72162022244582,1.,0.386070790323281));
#24526=CARTESIAN_POINT('Ctrl Pts',(1.71231062891398,1.,0.384119047314215));
#24527=CARTESIAN_POINT('Ctrl Pts',(1.7075470150345,1.,0.383122945602004));
#24528=CARTESIAN_POINT('',(2.11275013067528,0.,0.613422273260091));
#24529=CARTESIAN_POINT('Origin',(2.0698113262342,0.,0.745574324794401));
#24530=CARTESIAN_POINT('',(2.0698113262342,1.,0.745574324794401));
#24531=CARTESIAN_POINT('',(2.11275013067528,1.,0.613422273260091));
#24532=CARTESIAN_POINT('',(2.0698113262342,0.,0.745574324794401));
#24533=CARTESIAN_POINT('Ctrl Pts',(1.60662857109684,-1.,0.693717979106306));
#24534=CARTESIAN_POINT('Ctrl Pts',(1.60662857109684,1.,0.693717979106306));
#24535=CARTESIAN_POINT('Ctrl Pts',(1.61106790958151,-1.,0.695712097881194));
#24536=CARTESIAN_POINT('Ctrl Pts',(1.61106790958151,1.,0.695712097881194));
#24537=CARTESIAN_POINT('Ctrl Pts',(1.61974673472612,-1.,0.699605146405088));
#24538=CARTESIAN_POINT('Ctrl Pts',(1.61974673472612,1.,0.699605146405088));
#24539=CARTESIAN_POINT('Ctrl Pts',(1.63216541664676,-1.,0.705159151988319));
#24540=CARTESIAN_POINT('Ctrl Pts',(1.63216541664676,1.,0.705159151988319));
#24541=CARTESIAN_POINT('Ctrl Pts',(1.64752408832016,-1.,0.711993139355394));
#24542=CARTESIAN_POINT('Ctrl Pts',(1.64752408832016,1.,0.711993139355394));
#24543=CARTESIAN_POINT('Ctrl Pts',(1.6647288055568,-1.,0.719585433804282));
#24544=CARTESIAN_POINT('Ctrl Pts',(1.6647288055568,1.,0.719585433804282));
#24545=CARTESIAN_POINT('Ctrl Pts',(1.67996158455503,-1.,0.726235967997433));
#24546=CARTESIAN_POINT('Ctrl Pts',(1.67996158455503,1.,0.726235967997433));
#24547=CARTESIAN_POINT('Ctrl Pts',(1.69326921975743,-1.,0.731963238697195));
#24548=CARTESIAN_POINT('Ctrl Pts',(1.69326921975743,1.,0.731963238697195));
#24549=CARTESIAN_POINT('Ctrl Pts',(1.70473309006121,-1.,0.736799665724771));
#24550=CARTESIAN_POINT('Ctrl Pts',(1.70473309006121,1.,0.736799665724771));
#24551=CARTESIAN_POINT('Ctrl Pts',(1.71447789751927,-1.,0.740795162032088));
#24552=CARTESIAN_POINT('Ctrl Pts',(1.71447789751927,1.,0.740795162032088));
#24553=CARTESIAN_POINT('Ctrl Pts',(1.7226822991693,-1.,0.744021445433765));
#24554=CARTESIAN_POINT('Ctrl Pts',(1.7226822991693,1.,0.744021445433765));
#24555=CARTESIAN_POINT('Ctrl Pts',(1.72958533647399,-1.,0.746574710096437));
#24556=CARTESIAN_POINT('Ctrl Pts',(1.72958533647399,1.,0.746574710096437));
#24557=CARTESIAN_POINT('Ctrl Pts',(1.73550351679848,-1.,0.748582462954855));
#24558=CARTESIAN_POINT('Ctrl Pts',(1.73550351679848,1.,0.748582462954855));
#24559=CARTESIAN_POINT('Ctrl Pts',(1.74080458266705,-1.,0.750193435979541));
#24560=CARTESIAN_POINT('Ctrl Pts',(1.74080458266705,1.,0.750193435979541));
#24561=CARTESIAN_POINT('Ctrl Pts',(1.74585086852298,-1.,0.751555614163629));
#24562=CARTESIAN_POINT('Ctrl Pts',(1.74585086852298,1.,0.751555614163629));
#24563=CARTESIAN_POINT('Ctrl Pts',(1.75095139468809,-1.,0.752797683531377));
#24564=CARTESIAN_POINT('Ctrl Pts',(1.75095139468809,1.,0.752797683531377));
#24565=CARTESIAN_POINT('Ctrl Pts',(1.75631083600175,-1.,0.75400925402848));
#24566=CARTESIAN_POINT('Ctrl Pts',(1.75631083600175,1.,0.75400925402848));
#24567=CARTESIAN_POINT('Ctrl Pts',(1.7619781724032,-1.,0.755220979975262));
#24568=CARTESIAN_POINT('Ctrl Pts',(1.7619781724032,1.,0.755220979975262));
#24569=CARTESIAN_POINT('Ctrl Pts',(1.76789396003141,-1.,0.756421896028403));
#24570=CARTESIAN_POINT('Ctrl Pts',(1.76789396003141,1.,0.756421896028403));
#24571=CARTESIAN_POINT('Ctrl Pts',(1.77394167108342,-1.,0.757578264077238));
#24572=CARTESIAN_POINT('Ctrl Pts',(1.77394167108342,1.,0.757578264077238));
#24573=CARTESIAN_POINT('Ctrl Pts',(1.77999411220912,-1.,0.75865062667738));
#24574=CARTESIAN_POINT('Ctrl Pts',(1.77999411220912,1.,0.75865062667738));
#24575=CARTESIAN_POINT('Ctrl Pts',(1.78596964884526,-1.,0.759614401109868));
#24576=CARTESIAN_POINT('Ctrl Pts',(1.78596964884526,1.,0.759614401109868));
#24577=CARTESIAN_POINT('Ctrl Pts',(1.79185815610802,-1.,0.760469555880425));
#24578=CARTESIAN_POINT('Ctrl Pts',(1.79185815610802,1.,0.760469555880425));
#24579=CARTESIAN_POINT('Ctrl Pts',(1.79768986997735,-1.,0.761229695230359));
#24580=CARTESIAN_POINT('Ctrl Pts',(1.79768986997735,1.,0.761229695230359));
#24581=CARTESIAN_POINT('Ctrl Pts',(1.80351583877334,-1.,0.761915336443516));
#24582=CARTESIAN_POINT('Ctrl Pts',(1.80351583877334,1.,0.761915336443516));
#24583=CARTESIAN_POINT('Ctrl Pts',(1.80938551463989,-1.,0.762546129464036));
#24584=CARTESIAN_POINT('Ctrl Pts',(1.80938551463989,1.,0.762546129464036));
#24585=CARTESIAN_POINT('Ctrl Pts',(1.81532118405566,-1.,0.763132003836783));
#24586=CARTESIAN_POINT('Ctrl Pts',(1.81532118405566,1.,0.763132003836783));
#24587=CARTESIAN_POINT('Ctrl Pts',(1.82131873145297,-1.,0.763673465462854));
#24588=CARTESIAN_POINT('Ctrl Pts',(1.82131873145297,1.,0.763673465462854));
#24589=CARTESIAN_POINT('Ctrl Pts',(1.8273599120008,-1.,0.764165902606056));
#24590=CARTESIAN_POINT('Ctrl Pts',(1.8273599120008,1.,0.764165902606056));
#24591=CARTESIAN_POINT('Ctrl Pts',(1.8334207722714,-1.,0.764602549687846));
#24592=CARTESIAN_POINT('Ctrl Pts',(1.8334207722714,1.,0.764602549687846));
#24593=CARTESIAN_POINT('Ctrl Pts',(1.83948181064823,-1.,0.764978057881688));
#24594=CARTESIAN_POINT('Ctrl Pts',(1.83948181064823,1.,0.764978057881688));
#24595=CARTESIAN_POINT('Ctrl Pts',(1.8455369887591,-1.,0.765291664861972));
#24596=CARTESIAN_POINT('Ctrl Pts',(1.8455369887591,1.,0.765291664861972));
#24597=CARTESIAN_POINT('Ctrl Pts',(1.85158945130054,-1.,0.765545710619023));
#24598=CARTESIAN_POINT('Ctrl Pts',(1.85158945130054,1.,0.765545710619023));
#24599=CARTESIAN_POINT('Ctrl Pts',(1.85764741390391,-1.,0.765744212909305));
#24600=CARTESIAN_POINT('Ctrl Pts',(1.85764741390391,1.,0.765744212909305));
#24601=CARTESIAN_POINT('Ctrl Pts',(1.86372027063314,-1.,0.765891519092557));
#24602=CARTESIAN_POINT('Ctrl Pts',(1.86372027063314,1.,0.765891519092557));
#24603=CARTESIAN_POINT('Ctrl Pts',(1.86981398314345,-1.,0.765990708546112));
#24604=CARTESIAN_POINT('Ctrl Pts',(1.86981398314345,1.,0.765990708546112));
#24605=CARTESIAN_POINT('Ctrl Pts',(1.87592888967886,-1.,0.766042837036759));
#24606=CARTESIAN_POINT('Ctrl Pts',(1.87592888967886,1.,0.766042837036759));
#24607=CARTESIAN_POINT('Ctrl Pts',(1.88206215302561,-1.,0.766047794851869));
#24608=CARTESIAN_POINT('Ctrl Pts',(1.88206215302561,1.,0.766047794851869));
#24609=CARTESIAN_POINT('Ctrl Pts',(1.88820926433409,-1.,0.76600483706209));
#24610=CARTESIAN_POINT('Ctrl Pts',(1.88820926433409,1.,0.76600483706209));
#24611=CARTESIAN_POINT('Ctrl Pts',(1.89436577771389,-1.,0.765913193856979));
#24612=CARTESIAN_POINT('Ctrl Pts',(1.89436577771389,1.,0.765913193856979));
#24613=CARTESIAN_POINT('Ctrl Pts',(1.90052930393599,-1.,0.765772772593395));
#24614=CARTESIAN_POINT('Ctrl Pts',(1.90052930393599,1.,0.765772772593395));
#24615=CARTESIAN_POINT('Ctrl Pts',(1.90669961402362,-1.,0.765584196937937));
#24616=CARTESIAN_POINT('Ctrl Pts',(1.90669961402362,1.,0.765584196937937));
#24617=CARTESIAN_POINT('Ctrl Pts',(1.91287765805174,-1.,0.765348465884739));
#24618=CARTESIAN_POINT('Ctrl Pts',(1.91287765805174,1.,0.765348465884739));
#24619=CARTESIAN_POINT('Ctrl Pts',(1.91906491634197,-1.,0.765066729667095));
#24620=CARTESIAN_POINT('Ctrl Pts',(1.91906491634197,1.,0.765066729667095));
#24621=CARTESIAN_POINT('Ctrl Pts',(1.92526263537041,-1.,0.764740025488189));
#24622=CARTESIAN_POINT('Ctrl Pts',(1.92526263537041,1.,0.764740025488189));
#24623=CARTESIAN_POINT('Ctrl Pts',(1.93147105496367,-1.,0.76436901067389));
#24624=CARTESIAN_POINT('Ctrl Pts',(1.93147105496367,1.,0.76436901067389));
#24625=CARTESIAN_POINT('Ctrl Pts',(1.93768964875867,-1.,0.763954049121394));
#24626=CARTESIAN_POINT('Ctrl Pts',(1.93768964875867,1.,0.763954049121394));
#24627=CARTESIAN_POINT('Ctrl Pts',(1.94391746617626,-1.,0.763495333538581));
#24628=CARTESIAN_POINT('Ctrl Pts',(1.94391746617626,1.,0.763495333538581));
#24629=CARTESIAN_POINT('Ctrl Pts',(1.95015342590025,-1.,0.762992990878774));
#24630=CARTESIAN_POINT('Ctrl Pts',(1.95015342590025,1.,0.762992990878774));
#24631=CARTESIAN_POINT('Ctrl Pts',(1.95639665309893,-1.,0.762447203806264));
#24632=CARTESIAN_POINT('Ctrl Pts',(1.95639665309893,1.,0.762447203806264));
#24633=CARTESIAN_POINT('Ctrl Pts',(1.96264672744229,-1.,0.761858300014575));
#24634=CARTESIAN_POINT('Ctrl Pts',(1.96264672744229,1.,0.761858300014575));
#24635=CARTESIAN_POINT('Ctrl Pts',(1.96890351582545,-1.,0.761226690483986));
#24636=CARTESIAN_POINT('Ctrl Pts',(1.96890351582545,1.,0.761226690483986));
#24637=CARTESIAN_POINT('Ctrl Pts',(1.97516705321521,-1.,0.760552825409856));
#24638=CARTESIAN_POINT('Ctrl Pts',(1.97516705321521,1.,0.760552825409856));
#24639=CARTESIAN_POINT('Ctrl Pts',(1.98143741418156,-1.,0.759837147452135));
#24640=CARTESIAN_POINT('Ctrl Pts',(1.98143741418156,1.,0.759837147452135));
#24641=CARTESIAN_POINT('Ctrl Pts',(1.98771456680806,-1.,0.759080037802243));
#24642=CARTESIAN_POINT('Ctrl Pts',(1.98771456680806,1.,0.759080037802243));
#24643=CARTESIAN_POINT('Ctrl Pts',(1.9939983109871,-1.,0.758281796766377));
#24644=CARTESIAN_POINT('Ctrl Pts',(1.9939983109871,1.,0.758281796766377));
#24645=CARTESIAN_POINT('Ctrl Pts',(2.00028834739072,-1.,0.757442676862342));
#24646=CARTESIAN_POINT('Ctrl Pts',(2.00028834739072,1.,0.757442676862342));
#24647=CARTESIAN_POINT('Ctrl Pts',(2.00658431587682,-1.,0.756562904646496));
#24648=CARTESIAN_POINT('Ctrl Pts',(2.00658431587682,1.,0.756562904646496));
#24649=CARTESIAN_POINT('Ctrl Pts',(2.01288584328149,-1.,0.755642704958101));
#24650=CARTESIAN_POINT('Ctrl Pts',(2.01288584328149,1.,0.755642704958101));
#24651=CARTESIAN_POINT('Ctrl Pts',(2.01919259406003,-1.,0.75468233072352));
#24652=CARTESIAN_POINT('Ctrl Pts',(2.01919259406003,1.,0.75468233072352));
#24653=CARTESIAN_POINT('Ctrl Pts',(2.02550428623587,-1.,0.753682061113766));
#24654=CARTESIAN_POINT('Ctrl Pts',(2.02550428623587,1.,0.753682061113766));
#24655=CARTESIAN_POINT('Ctrl Pts',(2.03182068456467,-1.,0.752642180488104));
#24656=CARTESIAN_POINT('Ctrl Pts',(2.03182068456467,1.,0.752642180488104));
#24657=CARTESIAN_POINT('Ctrl Pts',(2.03814160092173,-1.,0.751562963361384));
#24658=CARTESIAN_POINT('Ctrl Pts',(2.03814160092173,1.,0.751562963361384));
#24659=CARTESIAN_POINT('Ctrl Pts',(2.04446689147754,-1.,0.750444657874758));
#24660=CARTESIAN_POINT('Ctrl Pts',(2.04446689147754,1.,0.750444657874758));
#24661=CARTESIAN_POINT('Ctrl Pts',(2.05079645591606,-1.,0.749287468663053));
#24662=CARTESIAN_POINT('Ctrl Pts',(2.05079645591606,1.,0.749287468663053));
#24663=CARTESIAN_POINT('Ctrl Pts',(2.05713023030263,-1.,0.748091554181101));
#24664=CARTESIAN_POINT('Ctrl Pts',(2.05713023030263,1.,0.748091554181101));
#24665=CARTESIAN_POINT('Ctrl Pts',(2.06220058927162,-1.,0.747103932785504));
#24666=CARTESIAN_POINT('Ctrl Pts',(2.06220058927162,1.,0.747103932785504));
#24667=CARTESIAN_POINT('Ctrl Pts',(2.06600523016401,-1.,0.746345871542696));
#24668=CARTESIAN_POINT('Ctrl Pts',(2.06600523016401,1.,0.746345871542696));
#24669=CARTESIAN_POINT('Ctrl Pts',(2.06854248895575,-1.,0.74583279137781));
#24670=CARTESIAN_POINT('Ctrl Pts',(2.06854248895575,1.,0.74583279137781));
#24671=CARTESIAN_POINT('Ctrl Pts',(2.0698113262342,-1.,0.745574324794401));
#24672=CARTESIAN_POINT('Ctrl Pts',(2.0698113262342,1.,0.745574324794401));
#24673=CARTESIAN_POINT('',(1.60662857109684,1.,0.693717979106306));
#24674=CARTESIAN_POINT('Ctrl Pts',(1.60662857109684,1.,0.693717979106306));
#24675=CARTESIAN_POINT('Ctrl Pts',(1.61106790958151,1.,0.695712097881194));
#24676=CARTESIAN_POINT('Ctrl Pts',(1.61974673472612,1.,0.699605146405088));
#24677=CARTESIAN_POINT('Ctrl Pts',(1.63216541664676,1.,0.705159151988319));
#24678=CARTESIAN_POINT('Ctrl Pts',(1.64752408832016,1.,0.711993139355394));
#24679=CARTESIAN_POINT('Ctrl Pts',(1.6647288055568,1.,0.719585433804282));
#24680=CARTESIAN_POINT('Ctrl Pts',(1.67996158455503,1.,0.726235967997433));
#24681=CARTESIAN_POINT('Ctrl Pts',(1.69326921975743,1.,0.731963238697195));
#24682=CARTESIAN_POINT('Ctrl Pts',(1.70473309006121,1.,0.736799665724771));
#24683=CARTESIAN_POINT('Ctrl Pts',(1.71447789751927,1.,0.740795162032088));
#24684=CARTESIAN_POINT('Ctrl Pts',(1.7226822991693,1.,0.744021445433765));
#24685=CARTESIAN_POINT('Ctrl Pts',(1.72958533647399,1.,0.746574710096437));
#24686=CARTESIAN_POINT('Ctrl Pts',(1.73550351679848,1.,0.748582462954855));
#24687=CARTESIAN_POINT('Ctrl Pts',(1.74080458266705,1.,0.750193435979541));
#24688=CARTESIAN_POINT('Ctrl Pts',(1.74585086852298,1.,0.751555614163629));
#24689=CARTESIAN_POINT('Ctrl Pts',(1.75095139468809,1.,0.752797683531377));
#24690=CARTESIAN_POINT('Ctrl Pts',(1.75631083600175,1.,0.75400925402848));
#24691=CARTESIAN_POINT('Ctrl Pts',(1.7619781724032,1.,0.755220979975262));
#24692=CARTESIAN_POINT('Ctrl Pts',(1.76789396003141,1.,0.756421896028403));
#24693=CARTESIAN_POINT('Ctrl Pts',(1.77394167108342,1.,0.757578264077238));
#24694=CARTESIAN_POINT('Ctrl Pts',(1.77999411220912,1.,0.75865062667738));
#24695=CARTESIAN_POINT('Ctrl Pts',(1.78596964884526,1.,0.759614401109868));
#24696=CARTESIAN_POINT('Ctrl Pts',(1.79185815610802,1.,0.760469555880425));
#24697=CARTESIAN_POINT('Ctrl Pts',(1.79768986997735,1.,0.761229695230359));
#24698=CARTESIAN_POINT('Ctrl Pts',(1.80351583877334,1.,0.761915336443516));
#24699=CARTESIAN_POINT('Ctrl Pts',(1.80938551463989,1.,0.762546129464036));
#24700=CARTESIAN_POINT('Ctrl Pts',(1.81532118405566,1.,0.763132003836783));
#24701=CARTESIAN_POINT('Ctrl Pts',(1.82131873145297,1.,0.763673465462854));
#24702=CARTESIAN_POINT('Ctrl Pts',(1.8273599120008,1.,0.764165902606056));
#24703=CARTESIAN_POINT('Ctrl Pts',(1.8334207722714,1.,0.764602549687846));
#24704=CARTESIAN_POINT('Ctrl Pts',(1.83948181064823,1.,0.764978057881688));
#24705=CARTESIAN_POINT('Ctrl Pts',(1.8455369887591,1.,0.765291664861972));
#24706=CARTESIAN_POINT('Ctrl Pts',(1.85158945130054,1.,0.765545710619023));
#24707=CARTESIAN_POINT('Ctrl Pts',(1.85764741390391,1.,0.765744212909305));
#24708=CARTESIAN_POINT('Ctrl Pts',(1.86372027063314,1.,0.765891519092557));
#24709=CARTESIAN_POINT('Ctrl Pts',(1.86981398314345,1.,0.765990708546112));
#24710=CARTESIAN_POINT('Ctrl Pts',(1.87592888967886,1.,0.766042837036759));
#24711=CARTESIAN_POINT('Ctrl Pts',(1.88206215302561,1.,0.766047794851869));
#24712=CARTESIAN_POINT('Ctrl Pts',(1.88820926433409,1.,0.76600483706209));
#24713=CARTESIAN_POINT('Ctrl Pts',(1.89436577771389,1.,0.765913193856979));
#24714=CARTESIAN_POINT('Ctrl Pts',(1.90052930393599,1.,0.765772772593395));
#24715=CARTESIAN_POINT('Ctrl Pts',(1.90669961402362,1.,0.765584196937937));
#24716=CARTESIAN_POINT('Ctrl Pts',(1.91287765805174,1.,0.765348465884739));
#24717=CARTESIAN_POINT('Ctrl Pts',(1.91906491634197,1.,0.765066729667095));
#24718=CARTESIAN_POINT('Ctrl Pts',(1.92526263537041,1.,0.764740025488189));
#24719=CARTESIAN_POINT('Ctrl Pts',(1.93147105496367,1.,0.76436901067389));
#24720=CARTESIAN_POINT('Ctrl Pts',(1.93768964875867,1.,0.763954049121394));
#24721=CARTESIAN_POINT('Ctrl Pts',(1.94391746617626,1.,0.763495333538581));
#24722=CARTESIAN_POINT('Ctrl Pts',(1.95015342590025,1.,0.762992990878774));
#24723=CARTESIAN_POINT('Ctrl Pts',(1.95639665309893,1.,0.762447203806264));
#24724=CARTESIAN_POINT('Ctrl Pts',(1.96264672744229,1.,0.761858300014575));
#24725=CARTESIAN_POINT('Ctrl Pts',(1.96890351582545,1.,0.761226690483986));
#24726=CARTESIAN_POINT('Ctrl Pts',(1.97516705321521,1.,0.760552825409856));
#24727=CARTESIAN_POINT('Ctrl Pts',(1.98143741418156,1.,0.759837147452135));
#24728=CARTESIAN_POINT('Ctrl Pts',(1.98771456680806,1.,0.759080037802243));
#24729=CARTESIAN_POINT('Ctrl Pts',(1.9939983109871,1.,0.758281796766377));
#24730=CARTESIAN_POINT('Ctrl Pts',(2.00028834739072,1.,0.757442676862342));
#24731=CARTESIAN_POINT('Ctrl Pts',(2.00658431587682,1.,0.756562904646496));
#24732=CARTESIAN_POINT('Ctrl Pts',(2.01288584328149,1.,0.755642704958101));
#24733=CARTESIAN_POINT('Ctrl Pts',(2.01919259406003,1.,0.75468233072352));
#24734=CARTESIAN_POINT('Ctrl Pts',(2.02550428623587,1.,0.753682061113766));
#24735=CARTESIAN_POINT('Ctrl Pts',(2.03182068456467,1.,0.752642180488104));
#24736=CARTESIAN_POINT('Ctrl Pts',(2.03814160092173,1.,0.751562963361384));
#24737=CARTESIAN_POINT('Ctrl Pts',(2.04446689147754,1.,0.750444657874758));
#24738=CARTESIAN_POINT('Ctrl Pts',(2.05079645591606,1.,0.749287468663053));
#24739=CARTESIAN_POINT('Ctrl Pts',(2.05713023030263,1.,0.748091554181101));
#24740=CARTESIAN_POINT('Ctrl Pts',(2.06220058927162,1.,0.747103932785504));
#24741=CARTESIAN_POINT('Ctrl Pts',(2.06600523016401,1.,0.746345871542696));
#24742=CARTESIAN_POINT('Ctrl Pts',(2.06854248895575,1.,0.74583279137781));
#24743=CARTESIAN_POINT('Ctrl Pts',(2.0698113262342,1.,0.745574324794401));
#24744=CARTESIAN_POINT('',(1.60662857109684,0.,0.693717979106305));
#24745=CARTESIAN_POINT('Origin',(0.,0.,0.));
#24746=CARTESIAN_POINT('',(1.5055822144029,1.,0.892032620296856));
#24747=CARTESIAN_POINT('Origin',(0.,1.,0.));
#24748=CARTESIAN_POINT('',(1.5055822144029,0.,0.892032620296855));
#24749=CARTESIAN_POINT('Ctrl Pts',(1.81978687191668,-1.,1.23627494547115));
#24750=CARTESIAN_POINT('Ctrl Pts',(1.81978687191668,1.,1.23627494547115));
#24751=CARTESIAN_POINT('Ctrl Pts',(1.81925017193666,-1.,1.23509651170476));
#24752=CARTESIAN_POINT('Ctrl Pts',(1.81925017193666,1.,1.23509651170476));
#24753=CARTESIAN_POINT('Ctrl Pts',(1.81817389921279,-1.,1.2327422452705));
#24754=CARTESIAN_POINT('Ctrl Pts',(1.81817389921279,1.,1.2327422452705));
#24755=CARTESIAN_POINT('Ctrl Pts',(1.8165508718364,-1.,1.2292186489137));
#24756=CARTESIAN_POINT('Ctrl Pts',(1.8165508718364,1.,1.2292186489137));
#24757=CARTESIAN_POINT('Ctrl Pts',(1.81436959210434,-1.,1.2245361330495));
#24758=CARTESIAN_POINT('Ctrl Pts',(1.81436959210434,1.,1.2245361330495));
#24759=CARTESIAN_POINT('Ctrl Pts',(1.81161420806656,-1.,1.21870906103557));
#24760=CARTESIAN_POINT('Ctrl Pts',(1.81161420806656,1.,1.21870906103557));
#24761=CARTESIAN_POINT('Ctrl Pts',(1.80882996917129,-1.,1.21290815708314));
#24762=CARTESIAN_POINT('Ctrl Pts',(1.80882996917129,1.,1.21290815708314));
#24763=CARTESIAN_POINT('Ctrl Pts',(1.80601678480707,-1.,1.20713356605475));
#24764=CARTESIAN_POINT('Ctrl Pts',(1.80601678480707,1.,1.20713356605475));
#24765=CARTESIAN_POINT('Ctrl Pts',(1.80317454838603,-1.,1.20138548938974));
#24766=CARTESIAN_POINT('Ctrl Pts',(1.80317454838603,1.,1.20138548938974));
#24767=CARTESIAN_POINT('Ctrl Pts',(1.80030314369879,-1.,1.19566418930242));
#24768=CARTESIAN_POINT('Ctrl Pts',(1.80030314369879,1.,1.19566418930242));
#24769=CARTESIAN_POINT('Ctrl Pts',(1.79740245923478,-1.,1.18996997934445));
#24770=CARTESIAN_POINT('Ctrl Pts',(1.79740245923478,1.,1.18996997934445));
#24771=CARTESIAN_POINT('Ctrl Pts',(1.79447240321515,-1.,1.18430321697432));
#24772=CARTESIAN_POINT('Ctrl Pts',(1.79447240321515,1.,1.18430321697432));
#24773=CARTESIAN_POINT('Ctrl Pts',(1.79151291552689,-1.,1.17866429440809));
#24774=CARTESIAN_POINT('Ctrl Pts',(1.79151291552689,1.,1.17866429440809));
#24775=CARTESIAN_POINT('Ctrl Pts',(1.78852398877616,-1.,1.17305363177328));
#24776=CARTESIAN_POINT('Ctrl Pts',(1.78852398877616,1.,1.17305363177328));
#24777=CARTESIAN_POINT('Ctrl Pts',(1.78550566040443,-1.,1.16747166312303));
#24778=CARTESIAN_POINT('Ctrl Pts',(1.78550566040443,1.,1.16747166312303));
#24779=CARTESIAN_POINT('Ctrl Pts',(1.78245795881009,-1.,1.16191881298499));
#24780=CARTESIAN_POINT('Ctrl Pts',(1.78245795881009,1.,1.16191881298499));
#24781=CARTESIAN_POINT('Ctrl Pts',(1.77938085564275,-1.,1.15639547194698));
#24782=CARTESIAN_POINT('Ctrl Pts',(1.77938085564275,1.,1.15639547194698));
#24783=CARTESIAN_POINT('Ctrl Pts',(1.7762742255701,-1.,1.15090197841515));
#24784=CARTESIAN_POINT('Ctrl Pts',(1.7762742255701,1.,1.15090197841515));
#24785=CARTESIAN_POINT('Ctrl Pts',(1.77313777896194,-1.,1.1454385822692));
#24786=CARTESIAN_POINT('Ctrl Pts',(1.77313777896194,1.,1.1454385822692));
#24787=CARTESIAN_POINT('Ctrl Pts',(1.76997111386769,-1.,1.14000548336975));
#24788=CARTESIAN_POINT('Ctrl Pts',(1.76997111386769,1.,1.14000548336975));
#24789=CARTESIAN_POINT('Ctrl Pts',(1.76677384551862,-1.,1.1346029180462));
#24790=CARTESIAN_POINT('Ctrl Pts',(1.76677384551862,1.,1.1346029180462));
#24791=CARTESIAN_POINT('Ctrl Pts',(1.7635457196617,-1.,1.12923123555075));
#24792=CARTESIAN_POINT('Ctrl Pts',(1.7635457196617,1.,1.12923123555075));
#24793=CARTESIAN_POINT('Ctrl Pts',(1.76028671825096,-1.,1.12389096855086));
#24794=CARTESIAN_POINT('Ctrl Pts',(1.76028671825096,1.,1.12389096855086));
#24795=CARTESIAN_POINT('Ctrl Pts',(1.75699720772105,-1.,1.11858293216763));
#24796=CARTESIAN_POINT('Ctrl Pts',(1.75699720772105,1.,1.11858293216763));
#24797=CARTESIAN_POINT('Ctrl Pts',(1.7536777209463,-1.,1.11330807582551));
#24798=CARTESIAN_POINT('Ctrl Pts',(1.7536777209463,1.,1.11330807582551));
#24799=CARTESIAN_POINT('Ctrl Pts',(1.7503286607592,-1.,1.10806728183007));
#24800=CARTESIAN_POINT('Ctrl Pts',(1.7503286607592,1.,1.10806728183007));
#24801=CARTESIAN_POINT('Ctrl Pts',(1.74695004214923,-1.,1.10286118991143));
#24802=CARTESIAN_POINT('Ctrl Pts',(1.74695004214923,1.,1.10286118991143));
#24803=CARTESIAN_POINT('Ctrl Pts',(1.74354119236208,-1.,1.09768999241226));
#24804=CARTESIAN_POINT('Ctrl Pts',(1.74354119236208,1.,1.09768999241226));
#24805=CARTESIAN_POINT('Ctrl Pts',(1.74010053962247,-1.,1.09255329056493));
#24806=CARTESIAN_POINT('Ctrl Pts',(1.74010053962247,1.,1.09255329056493));
#24807=CARTESIAN_POINT('Ctrl Pts',(1.73662628326091,-1.,1.08745056285427));
#24808=CARTESIAN_POINT('Ctrl Pts',(1.73662628326091,1.,1.08745056285427));
#24809=CARTESIAN_POINT('Ctrl Pts',(1.73311705663407,-1.,1.08238162784749));
#24810=CARTESIAN_POINT('Ctrl Pts',(1.73311705663407,1.,1.08238162784749));
#24811=CARTESIAN_POINT('Ctrl Pts',(1.72957248977424,-1.,1.0773470373727));
#24812=CARTESIAN_POINT('Ctrl Pts',(1.72957248977424,1.,1.0773470373727));
#24813=CARTESIAN_POINT('Ctrl Pts',(1.72599406198488,-1.,1.07234866990252));
#24814=CARTESIAN_POINT('Ctrl Pts',(1.72599406198488,1.,1.07234866990252));
#24815=CARTESIAN_POINT('Ctrl Pts',(1.72238500928453,-1.,1.06738966975462));
#24816=CARTESIAN_POINT('Ctrl Pts',(1.72238500928453,1.,1.06738966975462));
#24817=CARTESIAN_POINT('Ctrl Pts',(1.71874858456904,-1.,1.06247324680647));
#24818=CARTESIAN_POINT('Ctrl Pts',(1.71874858456904,1.,1.06247324680647));
#24819=CARTESIAN_POINT('Ctrl Pts',(1.7150865442702,-1.,1.05760163192479));
#24820=CARTESIAN_POINT('Ctrl Pts',(1.7150865442702,1.,1.05760163192479));
#24821=CARTESIAN_POINT('Ctrl Pts',(1.71139783543989,-1.,1.05277517202855));
#24822=CARTESIAN_POINT('Ctrl Pts',(1.71139783543989,1.,1.05277517202855));
#24823=CARTESIAN_POINT('Ctrl Pts',(1.70767646263649,-1.,1.04799085404995));
#24824=CARTESIAN_POINT('Ctrl Pts',(1.70767646263649,1.,1.04799085404995));
#24825=CARTESIAN_POINT('Ctrl Pts',(1.70391338707982,-1.,1.04324363334554));
#24826=CARTESIAN_POINT('Ctrl Pts',(1.70391338707982,1.,1.04324363334554));
#24827=CARTESIAN_POINT('Ctrl Pts',(1.70010052930962,-1.,1.03852922490789));
#24828=CARTESIAN_POINT('Ctrl Pts',(1.70010052930962,1.,1.03852922490789));
#24829=CARTESIAN_POINT('Ctrl Pts',(1.69623414782771,-1.,1.03384646003588));
#24830=CARTESIAN_POINT('Ctrl Pts',(1.69623414782771,1.,1.03384646003588));
#24831=CARTESIAN_POINT('Ctrl Pts',(1.69231840863458,-1.,1.02919977579147));
#24832=CARTESIAN_POINT('Ctrl Pts',(1.69231840863458,1.,1.02919977579147));
#24833=CARTESIAN_POINT('Ctrl Pts',(1.68836910178447,-1.,1.02460180535255));
#24834=CARTESIAN_POINT('Ctrl Pts',(1.68836910178447,1.,1.02460180535255));
#24835=CARTESIAN_POINT('Ctrl Pts',(1.68440578021706,-1.,1.02006795074201));
#24836=CARTESIAN_POINT('Ctrl Pts',(1.68440578021706,1.,1.02006795074201));
#24837=CARTESIAN_POINT('Ctrl Pts',(1.68044289894798,-1.,1.01561026162773));
#24838=CARTESIAN_POINT('Ctrl Pts',(1.68044289894798,1.,1.01561026162773));
#24839=CARTESIAN_POINT('Ctrl Pts',(1.67648246776464,-1.,1.01123236493511));
#24840=CARTESIAN_POINT('Ctrl Pts',(1.67648246776464,1.,1.01123236493511));
#24841=CARTESIAN_POINT('Ctrl Pts',(1.67250335383293,-1.,1.00692206696414));
#24842=CARTESIAN_POINT('Ctrl Pts',(1.67250335383293,1.,1.00692206696414));
#24843=CARTESIAN_POINT('Ctrl Pts',(1.66846059277303,-1.,1.00265091003727));
#24844=CARTESIAN_POINT('Ctrl Pts',(1.66846059277303,1.,1.00265091003727));
#24845=CARTESIAN_POINT('Ctrl Pts',(1.66430758030376,-1.,0.998389654952758));
#24846=CARTESIAN_POINT('Ctrl Pts',(1.66430758030376,1.,0.998389654952758));
#24847=CARTESIAN_POINT('Ctrl Pts',(1.66001553809947,-1.,0.994121836661306));
#24848=CARTESIAN_POINT('Ctrl Pts',(1.66001553809947,1.,0.994121836661306));
#24849=CARTESIAN_POINT('Ctrl Pts',(1.65559044289699,-1.,0.989855627854165));
#24850=CARTESIAN_POINT('Ctrl Pts',(1.65559044289699,1.,0.989855627854165));
#24851=CARTESIAN_POINT('Ctrl Pts',(1.65110016612638,-1.,0.985642622920821));
#24852=CARTESIAN_POINT('Ctrl Pts',(1.65110016612638,1.,0.985642622920821));
#24853=CARTESIAN_POINT('Ctrl Pts',(1.64665139190656,-1.,0.981562530939489));
#24854=CARTESIAN_POINT('Ctrl Pts',(1.64665139190656,1.,0.981562530939489));
#24855=CARTESIAN_POINT('Ctrl Pts',(1.64233990826687,-1.,0.977689794119417));
#24856=CARTESIAN_POINT('Ctrl Pts',(1.64233990826687,1.,0.977689794119417));
#24857=CARTESIAN_POINT('Ctrl Pts',(1.63820952658144,-1.,0.974066058287419));
#24858=CARTESIAN_POINT('Ctrl Pts',(1.63820952658144,1.,0.974066058287419));
#24859=CARTESIAN_POINT('Ctrl Pts',(1.63420665729798,-1.,0.970669715997509));
#24860=CARTESIAN_POINT('Ctrl Pts',(1.63420665729798,1.,0.970669715997509));
#24861=CARTESIAN_POINT('Ctrl Pts',(1.63013849959461,-1.,0.967387853230345));
#24862=CARTESIAN_POINT('Ctrl Pts',(1.63013849959461,1.,0.967387853230345));
#24863=CARTESIAN_POINT('Ctrl Pts',(1.62571930670187,-1.,0.964046107040536));
#24864=CARTESIAN_POINT('Ctrl Pts',(1.62571930670187,1.,0.964046107040536));
#24865=CARTESIAN_POINT('Ctrl Pts',(1.62061638140221,-1.,0.960438326101729));
#24866=CARTESIAN_POINT('Ctrl Pts',(1.62061638140221,1.,0.960438326101729));
#24867=CARTESIAN_POINT('Ctrl Pts',(1.61449324337085,-1.,0.956354422920671));
#24868=CARTESIAN_POINT('Ctrl Pts',(1.61449324337085,1.,0.956354422920671));
#24869=CARTESIAN_POINT('Ctrl Pts',(1.60706069896936,-1.,0.951613284356035));
#24870=CARTESIAN_POINT('Ctrl Pts',(1.60706069896936,1.,0.951613284356035));
#24871=CARTESIAN_POINT('Ctrl Pts',(1.59810042043673,-1.,0.946078063315257));
#24872=CARTESIAN_POINT('Ctrl Pts',(1.59810042043673,1.,0.946078063315257));
#24873=CARTESIAN_POINT('Ctrl Pts',(1.58744937487176,-1.,0.939646377893399));
#24874=CARTESIAN_POINT('Ctrl Pts',(1.58744937487176,1.,0.939646377893399));
#24875=CARTESIAN_POINT('Ctrl Pts',(1.57499388382243,-1.,0.932246680108685));
#24876=CARTESIAN_POINT('Ctrl Pts',(1.57499388382243,1.,0.932246680108685));
#24877=CARTESIAN_POINT('Ctrl Pts',(1.56065988578893,-1.,0.923832188944341));
#24878=CARTESIAN_POINT('Ctrl Pts',(1.56065988578893,1.,0.923832188944341));
#24879=CARTESIAN_POINT('Ctrl Pts',(1.54440491149498,-1.,0.914375919026456));
#24880=CARTESIAN_POINT('Ctrl Pts',(1.54440491149498,1.,0.914375919026456));
#24881=CARTESIAN_POINT('Ctrl Pts',(1.52984849887993,-1.,0.905967409625651));
#24882=CARTESIAN_POINT('Ctrl Pts',(1.52984849887993,1.,0.905967409625651));
#24883=CARTESIAN_POINT('Ctrl Pts',(1.51805569590094,-1.,0.899185047483511));
#24884=CARTESIAN_POINT('Ctrl Pts',(1.51805569590094,1.,0.899185047483511));
#24885=CARTESIAN_POINT('Ctrl Pts',(1.50980486806688,-1.,0.894452006964544));
#24886=CARTESIAN_POINT('Ctrl Pts',(1.50980486806688,1.,0.894452006964544));
#24887=CARTESIAN_POINT('Ctrl Pts',(1.5055822144029,-1.,0.892032620296856));
#24888=CARTESIAN_POINT('Ctrl Pts',(1.5055822144029,1.,0.892032620296856));
#24889=CARTESIAN_POINT('',(1.81978687191668,1.,1.23627494547115));
#24890=CARTESIAN_POINT('Ctrl Pts',(1.81978687191668,1.,1.23627494547115));
#24891=CARTESIAN_POINT('Ctrl Pts',(1.81925017193666,1.,1.23509651170476));
#24892=CARTESIAN_POINT('Ctrl Pts',(1.81817389921279,1.,1.2327422452705));
#24893=CARTESIAN_POINT('Ctrl Pts',(1.8165508718364,1.,1.2292186489137));
#24894=CARTESIAN_POINT('Ctrl Pts',(1.81436959210434,1.,1.2245361330495));
#24895=CARTESIAN_POINT('Ctrl Pts',(1.81161420806656,1.,1.21870906103557));
#24896=CARTESIAN_POINT('Ctrl Pts',(1.80882996917129,1.,1.21290815708314));
#24897=CARTESIAN_POINT('Ctrl Pts',(1.80601678480707,1.,1.20713356605475));
#24898=CARTESIAN_POINT('Ctrl Pts',(1.80317454838603,1.,1.20138548938974));
#24899=CARTESIAN_POINT('Ctrl Pts',(1.80030314369879,1.,1.19566418930242));
#24900=CARTESIAN_POINT('Ctrl Pts',(1.79740245923478,1.,1.18996997934445));
#24901=CARTESIAN_POINT('Ctrl Pts',(1.79447240321515,1.,1.18430321697432));
#24902=CARTESIAN_POINT('Ctrl Pts',(1.79151291552689,1.,1.17866429440809));
#24903=CARTESIAN_POINT('Ctrl Pts',(1.78852398877616,1.,1.17305363177328));
#24904=CARTESIAN_POINT('Ctrl Pts',(1.78550566040443,1.,1.16747166312303));
#24905=CARTESIAN_POINT('Ctrl Pts',(1.78245795881009,1.,1.16191881298499));
#24906=CARTESIAN_POINT('Ctrl Pts',(1.77938085564275,1.,1.15639547194698));
#24907=CARTESIAN_POINT('Ctrl Pts',(1.7762742255701,1.,1.15090197841515));
#24908=CARTESIAN_POINT('Ctrl Pts',(1.77313777896194,1.,1.1454385822692));
#24909=CARTESIAN_POINT('Ctrl Pts',(1.76997111386769,1.,1.14000548336975));
#24910=CARTESIAN_POINT('Ctrl Pts',(1.76677384551862,1.,1.1346029180462));
#24911=CARTESIAN_POINT('Ctrl Pts',(1.7635457196617,1.,1.12923123555075));
#24912=CARTESIAN_POINT('Ctrl Pts',(1.76028671825096,1.,1.12389096855086));
#24913=CARTESIAN_POINT('Ctrl Pts',(1.75699720772105,1.,1.11858293216763));
#24914=CARTESIAN_POINT('Ctrl Pts',(1.7536777209463,1.,1.11330807582551));
#24915=CARTESIAN_POINT('Ctrl Pts',(1.7503286607592,1.,1.10806728183007));
#24916=CARTESIAN_POINT('Ctrl Pts',(1.74695004214923,1.,1.10286118991143));
#24917=CARTESIAN_POINT('Ctrl Pts',(1.74354119236208,1.,1.09768999241226));
#24918=CARTESIAN_POINT('Ctrl Pts',(1.74010053962247,1.,1.09255329056493));
#24919=CARTESIAN_POINT('Ctrl Pts',(1.73662628326091,1.,1.08745056285427));
#24920=CARTESIAN_POINT('Ctrl Pts',(1.73311705663407,1.,1.08238162784749));
#24921=CARTESIAN_POINT('Ctrl Pts',(1.72957248977424,1.,1.0773470373727));
#24922=CARTESIAN_POINT('Ctrl Pts',(1.72599406198488,1.,1.07234866990252));
#24923=CARTESIAN_POINT('Ctrl Pts',(1.72238500928453,1.,1.06738966975462));
#24924=CARTESIAN_POINT('Ctrl Pts',(1.71874858456904,1.,1.06247324680647));
#24925=CARTESIAN_POINT('Ctrl Pts',(1.7150865442702,1.,1.05760163192479));
#24926=CARTESIAN_POINT('Ctrl Pts',(1.71139783543989,1.,1.05277517202855));
#24927=CARTESIAN_POINT('Ctrl Pts',(1.70767646263649,1.,1.04799085404995));
#24928=CARTESIAN_POINT('Ctrl Pts',(1.70391338707982,1.,1.04324363334554));
#24929=CARTESIAN_POINT('Ctrl Pts',(1.70010052930962,1.,1.03852922490789));
#24930=CARTESIAN_POINT('Ctrl Pts',(1.69623414782771,1.,1.03384646003588));
#24931=CARTESIAN_POINT('Ctrl Pts',(1.69231840863458,1.,1.02919977579147));
#24932=CARTESIAN_POINT('Ctrl Pts',(1.68836910178447,1.,1.02460180535255));
#24933=CARTESIAN_POINT('Ctrl Pts',(1.68440578021706,1.,1.02006795074201));
#24934=CARTESIAN_POINT('Ctrl Pts',(1.68044289894798,1.,1.01561026162773));
#24935=CARTESIAN_POINT('Ctrl Pts',(1.67648246776464,1.,1.01123236493511));
#24936=CARTESIAN_POINT('Ctrl Pts',(1.67250335383293,1.,1.00692206696414));
#24937=CARTESIAN_POINT('Ctrl Pts',(1.66846059277303,1.,1.00265091003727));
#24938=CARTESIAN_POINT('Ctrl Pts',(1.66430758030376,1.,0.998389654952758));
#24939=CARTESIAN_POINT('Ctrl Pts',(1.66001553809947,1.,0.994121836661306));
#24940=CARTESIAN_POINT('Ctrl Pts',(1.65559044289699,1.,0.989855627854165));
#24941=CARTESIAN_POINT('Ctrl Pts',(1.65110016612638,1.,0.985642622920821));
#24942=CARTESIAN_POINT('Ctrl Pts',(1.64665139190656,1.,0.981562530939489));
#24943=CARTESIAN_POINT('Ctrl Pts',(1.64233990826687,1.,0.977689794119417));
#24944=CARTESIAN_POINT('Ctrl Pts',(1.63820952658144,1.,0.974066058287419));
#24945=CARTESIAN_POINT('Ctrl Pts',(1.63420665729798,1.,0.970669715997509));
#24946=CARTESIAN_POINT('Ctrl Pts',(1.63013849959461,1.,0.967387853230345));
#24947=CARTESIAN_POINT('Ctrl Pts',(1.62571930670187,1.,0.964046107040536));
#24948=CARTESIAN_POINT('Ctrl Pts',(1.62061638140221,1.,0.960438326101729));
#24949=CARTESIAN_POINT('Ctrl Pts',(1.61449324337085,1.,0.956354422920671));
#24950=CARTESIAN_POINT('Ctrl Pts',(1.60706069896936,1.,0.951613284356035));
#24951=CARTESIAN_POINT('Ctrl Pts',(1.59810042043673,1.,0.946078063315257));
#24952=CARTESIAN_POINT('Ctrl Pts',(1.58744937487176,1.,0.939646377893399));
#24953=CARTESIAN_POINT('Ctrl Pts',(1.57499388382243,1.,0.932246680108685));
#24954=CARTESIAN_POINT('Ctrl Pts',(1.56065988578893,1.,0.923832188944341));
#24955=CARTESIAN_POINT('Ctrl Pts',(1.54440491149498,1.,0.914375919026456));
#24956=CARTESIAN_POINT('Ctrl Pts',(1.52984849887993,1.,0.905967409625651));
#24957=CARTESIAN_POINT('Ctrl Pts',(1.51805569590094,1.,0.899185047483511));
#24958=CARTESIAN_POINT('Ctrl Pts',(1.50980486806688,1.,0.894452006964544));
#24959=CARTESIAN_POINT('Ctrl Pts',(1.5055822144029,1.,0.892032620296856));
#24960=CARTESIAN_POINT('',(1.81978687191668,0.,1.23627494547115));
#24961=CARTESIAN_POINT('Origin',(1.73811241238545,0.,1.34869019493419));
#24962=CARTESIAN_POINT('',(1.73811241238545,1.,1.34869019493419));
#24963=CARTESIAN_POINT('',(1.81978687191668,1.,1.23627494547115));
#24964=CARTESIAN_POINT('',(1.73811241238545,0.,1.34869019493419));
#24965=CARTESIAN_POINT('Ctrl Pts',(1.31362392696032,-1.,1.15624053661742));
#24966=CARTESIAN_POINT('Ctrl Pts',(1.31362392696032,1.,1.15624053661742));
#24967=CARTESIAN_POINT('Ctrl Pts',(1.31722977216397,-1.,1.15950888730809));
#24968=CARTESIAN_POINT('Ctrl Pts',(1.31722977216397,1.,1.15950888730809));
#24969=CARTESIAN_POINT('Ctrl Pts',(1.32428080721772,-1.,1.16589330093588));
#24970=CARTESIAN_POINT('Ctrl Pts',(1.32428080721772,1.,1.16589330093588));
#24971=CARTESIAN_POINT('Ctrl Pts',(1.33437539347008,-1.,1.17501305789857));
#24972=CARTESIAN_POINT('Ctrl Pts',(1.33437539347008,1.,1.17501305789857));
#24973=CARTESIAN_POINT('Ctrl Pts',(1.34687054001093,-1.,1.18625865667441));
#24974=CARTESIAN_POINT('Ctrl Pts',(1.34687054001093,1.,1.18625865667441));
#24975=CARTESIAN_POINT('Ctrl Pts',(1.36088705043885,-1.,1.1987959077932));
#24976=CARTESIAN_POINT('Ctrl Pts',(1.36088705043885,1.,1.1987959077932));
#24977=CARTESIAN_POINT('Ctrl Pts',(1.37331915607905,-1.,1.20982812925645));
#24978=CARTESIAN_POINT('Ctrl Pts',(1.37331915607905,1.,1.20982812925645));
#24979=CARTESIAN_POINT('Ctrl Pts',(1.38420564527715,-1.,1.21938737280852));
#24980=CARTESIAN_POINT('Ctrl Pts',(1.38420564527715,1.,1.21938737280852));
#24981=CARTESIAN_POINT('Ctrl Pts',(1.39361389568796,-1.,1.22752961899387));
#24982=CARTESIAN_POINT('Ctrl Pts',(1.39361389568796,1.,1.22752961899387));
#24983=CARTESIAN_POINT('Ctrl Pts',(1.40164708206106,-1.,1.23434087290423));
#24984=CARTESIAN_POINT('Ctrl Pts',(1.40164708206106,1.,1.23434087290423));
#24985=CARTESIAN_POINT('Ctrl Pts',(1.40845295531283,-1.,1.23994455029534));
#24986=CARTESIAN_POINT('Ctrl Pts',(1.40845295531283,1.,1.23994455029534));
#24987=CARTESIAN_POINT('Ctrl Pts',(1.41422913175179,-1.,1.24450600513056));
#24988=CARTESIAN_POINT('Ctrl Pts',(1.41422913175179,1.,1.24450600513056));
#24989=CARTESIAN_POINT('Ctrl Pts',(1.41923722596025,-1.,1.24824430986571));
#24990=CARTESIAN_POINT('Ctrl Pts',(1.41923722596025,1.,1.24824430986571));
#24991=CARTESIAN_POINT('Ctrl Pts',(1.42378102115575,-1.,1.2514145557001));
#24992=CARTESIAN_POINT('Ctrl Pts',(1.42378102115575,1.,1.2514145557001));
#24993=CARTESIAN_POINT('Ctrl Pts',(1.42815938799387,-1.,1.25426945222639));
#24994=CARTESIAN_POINT('Ctrl Pts',(1.42815938799387,1.,1.25426945222639));
#24995=CARTESIAN_POINT('Ctrl Pts',(1.43262645609691,-1.,1.25702687965755));
#24996=CARTESIAN_POINT('Ctrl Pts',(1.43262645609691,1.,1.25702687965755));
#24997=CARTESIAN_POINT('Ctrl Pts',(1.43734919180847,-1.,1.25983531012005));
#24998=CARTESIAN_POINT('Ctrl Pts',(1.43734919180847,1.,1.25983531012005));
#24999=CARTESIAN_POINT('Ctrl Pts',(1.44236470511303,-1.,1.26273903323859));
#25000=CARTESIAN_POINT('Ctrl Pts',(1.44236470511303,1.,1.26273903323859));
#25001=CARTESIAN_POINT('Ctrl Pts',(1.44761985001662,-1.,1.26570925118868));
#25002=CARTESIAN_POINT('Ctrl Pts',(1.44761985001662,1.,1.26570925118868));
#25003=CARTESIAN_POINT('Ctrl Pts',(1.45301422764247,-1.,1.2686778680489));
#25004=CARTESIAN_POINT('Ctrl Pts',(1.45301422764247,1.,1.2686778680489));
#25005=CARTESIAN_POINT('Ctrl Pts',(1.45843906294697,-1.,1.27156805265289));
#25006=CARTESIAN_POINT('Ctrl Pts',(1.45843906294697,1.,1.27156805265289));
#25007=CARTESIAN_POINT('Ctrl Pts',(1.46382431332476,-1.,1.27433119897822));
#25008=CARTESIAN_POINT('Ctrl Pts',(1.46382431332476,1.,1.27433119897822));
#25009=CARTESIAN_POINT('Ctrl Pts',(1.46916035917133,-1.,1.2769641483109));
#25010=CARTESIAN_POINT('Ctrl Pts',(1.46916035917133,1.,1.2769641483109));
#25011=CARTESIAN_POINT('Ctrl Pts',(1.4744717526707,-1.,1.2794891824849));
#25012=CARTESIAN_POINT('Ctrl Pts',(1.4744717526707,1.,1.2794891824849));
#25013=CARTESIAN_POINT('Ctrl Pts',(1.47980070347095,-1.,1.28194158939517));
#25014=CARTESIAN_POINT('Ctrl Pts',(1.47980070347095,1.,1.28194158939517));
#25015=CARTESIAN_POINT('Ctrl Pts',(1.4851881711891,-1.,1.28435533880201));
#25016=CARTESIAN_POINT('Ctrl Pts',(1.4851881711891,1.,1.28435533880201));
#25017=CARTESIAN_POINT('Ctrl Pts',(1.4906522831278,-1.,1.2867467611644));
#25018=CARTESIAN_POINT('Ctrl Pts',(1.4906522831278,1.,1.2867467611644));
#25019=CARTESIAN_POINT('Ctrl Pts',(1.49618896881754,-1.,1.28911506584254));
#25020=CARTESIAN_POINT('Ctrl Pts',(1.49618896881754,1.,1.28911506584254));
#25021=CARTESIAN_POINT('Ctrl Pts',(1.50178230149776,-1.,1.29145022885181));
#25022=CARTESIAN_POINT('Ctrl Pts',(1.50178230149776,1.,1.29145022885181));
#25023=CARTESIAN_POINT('Ctrl Pts',(1.50741159078365,-1.,1.29373841372842));
#25024=CARTESIAN_POINT('Ctrl Pts',(1.50741159078365,1.,1.29373841372842));
#25025=CARTESIAN_POINT('Ctrl Pts',(1.51305994241402,-1.,1.29596850710509));
#25026=CARTESIAN_POINT('Ctrl Pts',(1.51305994241402,1.,1.29596850710509));
#25027=CARTESIAN_POINT('Ctrl Pts',(1.51872184912724,-1.,1.29813791800747));
#25028=CARTESIAN_POINT('Ctrl Pts',(1.51872184912724,1.,1.29813791800747));
#25029=CARTESIAN_POINT('Ctrl Pts',(1.52439957861062,-1.,1.30024984366328));
#25030=CARTESIAN_POINT('Ctrl Pts',(1.52439957861062,1.,1.30024984366328));
#25031=CARTESIAN_POINT('Ctrl Pts',(1.53009970283891,-1.,1.30231064395568));
#25032=CARTESIAN_POINT('Ctrl Pts',(1.53009970283891,1.,1.30231064395568));
#25033=CARTESIAN_POINT('Ctrl Pts',(1.53582981268977,-1.,1.30432735639489));
#25034=CARTESIAN_POINT('Ctrl Pts',(1.53582981268977,1.,1.30432735639489));
#25035=CARTESIAN_POINT('Ctrl Pts',(1.54159462645432,-1.,1.30630475189556));
#25036=CARTESIAN_POINT('Ctrl Pts',(1.54159462645432,1.,1.30630475189556));
#25037=CARTESIAN_POINT('Ctrl Pts',(1.54739413957185,-1.,1.30824393907473));
#25038=CARTESIAN_POINT('Ctrl Pts',(1.54739413957185,1.,1.30824393907473));
#25039=CARTESIAN_POINT('Ctrl Pts',(1.55322568759481,-1.,1.31014393684222));
#25040=CARTESIAN_POINT('Ctrl Pts',(1.55322568759481,1.,1.31014393684222));
#25041=CARTESIAN_POINT('Ctrl Pts',(1.55908521254821,-1.,1.31200264341696));
#25042=CARTESIAN_POINT('Ctrl Pts',(1.55908521254821,1.,1.31200264341696));
#25043=CARTESIAN_POINT('Ctrl Pts',(1.56496872402353,-1.,1.31381795281002));
#25044=CARTESIAN_POINT('Ctrl Pts',(1.56496872402353,1.,1.31381795281002));
#25045=CARTESIAN_POINT('Ctrl Pts',(1.57087397835723,-1.,1.31558903860016));
#25046=CARTESIAN_POINT('Ctrl Pts',(1.57087397835723,1.,1.31558903860016));
#25047=CARTESIAN_POINT('Ctrl Pts',(1.5768005650559,-1.,1.31731642317187));
#25048=CARTESIAN_POINT('Ctrl Pts',(1.5768005650559,1.,1.31731642317187));
#25049=CARTESIAN_POINT('Ctrl Pts',(1.58274907898834,-1.,1.31900135021432));
#25050=CARTESIAN_POINT('Ctrl Pts',(1.58274907898834,1.,1.31900135021432));
#25051=CARTESIAN_POINT('Ctrl Pts',(1.58872057258245,-1.,1.32064537110892));
#25052=CARTESIAN_POINT('Ctrl Pts',(1.58872057258245,1.,1.32064537110892));
#25053=CARTESIAN_POINT('Ctrl Pts',(1.59471591079403,-1.,1.32224985747682));
#25054=CARTESIAN_POINT('Ctrl Pts',(1.59471591079403,1.,1.32224985747682));
#25055=CARTESIAN_POINT('Ctrl Pts',(1.60073511858687,-1.,1.32381550858256));
#25056=CARTESIAN_POINT('Ctrl Pts',(1.60073511858687,1.,1.32381550858256));
#25057=CARTESIAN_POINT('Ctrl Pts',(1.60677758290954,-1.,1.32534250785782));
#25058=CARTESIAN_POINT('Ctrl Pts',(1.60677758290954,1.,1.32534250785782));
#25059=CARTESIAN_POINT('Ctrl Pts',(1.6128423401575,-1.,1.32683074483356));
#25060=CARTESIAN_POINT('Ctrl Pts',(1.6128423401575,1.,1.32683074483356));
#25061=CARTESIAN_POINT('Ctrl Pts',(1.61892832270724,-1.,1.32828000610449));
#25062=CARTESIAN_POINT('Ctrl Pts',(1.61892832270724,1.,1.32828000610449));
#25063=CARTESIAN_POINT('Ctrl Pts',(1.62503464209797,-1.,1.3296901950568));
#25064=CARTESIAN_POINT('Ctrl Pts',(1.62503464209797,1.,1.3296901950568));
#25065=CARTESIAN_POINT('Ctrl Pts',(1.63116079730923,-1.,1.33106149345645));
#25066=CARTESIAN_POINT('Ctrl Pts',(1.63116079730923,1.,1.33106149345645));
#25067=CARTESIAN_POINT('Ctrl Pts',(1.63730653475089,-1.,1.33239425103724));
#25068=CARTESIAN_POINT('Ctrl Pts',(1.63730653475089,1.,1.33239425103724));
#25069=CARTESIAN_POINT('Ctrl Pts',(1.6434717485603,-1.,1.33368890676572));
#25070=CARTESIAN_POINT('Ctrl Pts',(1.6434717485603,1.,1.33368890676572));
#25071=CARTESIAN_POINT('Ctrl Pts',(1.6496563728683,-1.,1.33494590467993));
#25072=CARTESIAN_POINT('Ctrl Pts',(1.6496563728683,1.,1.33494590467993));
#25073=CARTESIAN_POINT('Ctrl Pts',(1.65586025952593,-1.,1.33616559745172));
#25074=CARTESIAN_POINT('Ctrl Pts',(1.65586025952593,1.,1.33616559745172));
#25075=CARTESIAN_POINT('Ctrl Pts',(1.66208312541983,-1.,1.33734820885262));
#25076=CARTESIAN_POINT('Ctrl Pts',(1.66208312541983,1.,1.33734820885262));
#25077=CARTESIAN_POINT('Ctrl Pts',(1.66832460783989,-1.,1.33849388654388));
#25078=CARTESIAN_POINT('Ctrl Pts',(1.66832460783989,1.,1.33849388654388));
#25079=CARTESIAN_POINT('Ctrl Pts',(1.67458429426086,-1.,1.3396027347034));
#25080=CARTESIAN_POINT('Ctrl Pts',(1.67458429426086,1.,1.3396027347034));
#25081=CARTESIAN_POINT('Ctrl Pts',(1.68086176030362,-1.,1.34067485185203));
#25082=CARTESIAN_POINT('Ctrl Pts',(1.68086176030362,1.,1.34067485185203));
#25083=CARTESIAN_POINT('Ctrl Pts',(1.68715660868764,-1.,1.341710374848));
#25084=CARTESIAN_POINT('Ctrl Pts',(1.68715660868764,1.,1.341710374848));
#25085=CARTESIAN_POINT('Ctrl Pts',(1.6934684849687,-1.,1.34270948206319));
#25086=CARTESIAN_POINT('Ctrl Pts',(1.6934684849687,1.,1.34270948206319));
#25087=CARTESIAN_POINT('Ctrl Pts',(1.69979707754427,-1.,1.34367237124483));
#25088=CARTESIAN_POINT('Ctrl Pts',(1.69979707754427,1.,1.34367237124483));
#25089=CARTESIAN_POINT('Ctrl Pts',(1.70614212266738,-1.,1.34459924533831));
#25090=CARTESIAN_POINT('Ctrl Pts',(1.70614212266738,1.,1.34459924533831));
#25091=CARTESIAN_POINT('Ctrl Pts',(1.71250340686822,-1.,1.34549029589416));
#25092=CARTESIAN_POINT('Ctrl Pts',(1.71250340686822,1.,1.34549029589416));
#25093=CARTESIAN_POINT('Ctrl Pts',(1.7188807715049,-1.,1.34634568653227));
#25094=CARTESIAN_POINT('Ctrl Pts',(1.7188807715049,1.,1.34634568653227));
#25095=CARTESIAN_POINT('Ctrl Pts',(1.72527410680674,-1.,1.34716554819527));
#25096=CARTESIAN_POINT('Ctrl Pts',(1.72527410680674,1.,1.34716554819527));
#25097=CARTESIAN_POINT('Ctrl Pts',(1.7304014965394,-1.,1.34779309152035));
#25098=CARTESIAN_POINT('Ctrl Pts',(1.7304014965394,1.,1.34779309152035));
#25099=CARTESIAN_POINT('Ctrl Pts',(1.73425417885907,-1.,1.34824783112887));
#25100=CARTESIAN_POINT('Ctrl Pts',(1.73425417885907,1.,1.34824783112887));
#25101=CARTESIAN_POINT('Ctrl Pts',(1.73682580585691,-1.,1.34854391898045));
#25102=CARTESIAN_POINT('Ctrl Pts',(1.73682580585691,1.,1.34854391898045));
#25103=CARTESIAN_POINT('Ctrl Pts',(1.73811241238545,-1.,1.34869019493419));
#25104=CARTESIAN_POINT('Ctrl Pts',(1.73811241238545,1.,1.34869019493419));
#25105=CARTESIAN_POINT('',(1.31362392696032,1.,1.15624053661742));
#25106=CARTESIAN_POINT('Ctrl Pts',(1.31362392696032,1.,1.15624053661742));
#25107=CARTESIAN_POINT('Ctrl Pts',(1.31722977216397,1.,1.15950888730809));
#25108=CARTESIAN_POINT('Ctrl Pts',(1.32428080721772,1.,1.16589330093588));
#25109=CARTESIAN_POINT('Ctrl Pts',(1.33437539347008,1.,1.17501305789857));
#25110=CARTESIAN_POINT('Ctrl Pts',(1.34687054001093,1.,1.18625865667441));
#25111=CARTESIAN_POINT('Ctrl Pts',(1.36088705043885,1.,1.1987959077932));
#25112=CARTESIAN_POINT('Ctrl Pts',(1.37331915607905,1.,1.20982812925645));
#25113=CARTESIAN_POINT('Ctrl Pts',(1.38420564527715,1.,1.21938737280852));
#25114=CARTESIAN_POINT('Ctrl Pts',(1.39361389568796,1.,1.22752961899387));
#25115=CARTESIAN_POINT('Ctrl Pts',(1.40164708206106,1.,1.23434087290423));
#25116=CARTESIAN_POINT('Ctrl Pts',(1.40845295531283,1.,1.23994455029534));
#25117=CARTESIAN_POINT('Ctrl Pts',(1.41422913175179,1.,1.24450600513056));
#25118=CARTESIAN_POINT('Ctrl Pts',(1.41923722596025,1.,1.24824430986571));
#25119=CARTESIAN_POINT('Ctrl Pts',(1.42378102115575,1.,1.2514145557001));
#25120=CARTESIAN_POINT('Ctrl Pts',(1.42815938799387,1.,1.25426945222639));
#25121=CARTESIAN_POINT('Ctrl Pts',(1.43262645609691,1.,1.25702687965755));
#25122=CARTESIAN_POINT('Ctrl Pts',(1.43734919180847,1.,1.25983531012005));
#25123=CARTESIAN_POINT('Ctrl Pts',(1.44236470511303,1.,1.26273903323859));
#25124=CARTESIAN_POINT('Ctrl Pts',(1.44761985001662,1.,1.26570925118868));
#25125=CARTESIAN_POINT('Ctrl Pts',(1.45301422764247,1.,1.2686778680489));
#25126=CARTESIAN_POINT('Ctrl Pts',(1.45843906294697,1.,1.27156805265289));
#25127=CARTESIAN_POINT('Ctrl Pts',(1.46382431332476,1.,1.27433119897822));
#25128=CARTESIAN_POINT('Ctrl Pts',(1.46916035917133,1.,1.2769641483109));
#25129=CARTESIAN_POINT('Ctrl Pts',(1.4744717526707,1.,1.2794891824849));
#25130=CARTESIAN_POINT('Ctrl Pts',(1.47980070347095,1.,1.28194158939517));
#25131=CARTESIAN_POINT('Ctrl Pts',(1.4851881711891,1.,1.28435533880201));
#25132=CARTESIAN_POINT('Ctrl Pts',(1.4906522831278,1.,1.2867467611644));
#25133=CARTESIAN_POINT('Ctrl Pts',(1.49618896881754,1.,1.28911506584254));
#25134=CARTESIAN_POINT('Ctrl Pts',(1.50178230149776,1.,1.29145022885181));
#25135=CARTESIAN_POINT('Ctrl Pts',(1.50741159078365,1.,1.29373841372842));
#25136=CARTESIAN_POINT('Ctrl Pts',(1.51305994241402,1.,1.29596850710509));
#25137=CARTESIAN_POINT('Ctrl Pts',(1.51872184912724,1.,1.29813791800747));
#25138=CARTESIAN_POINT('Ctrl Pts',(1.52439957861062,1.,1.30024984366328));
#25139=CARTESIAN_POINT('Ctrl Pts',(1.53009970283891,1.,1.30231064395568));
#25140=CARTESIAN_POINT('Ctrl Pts',(1.53582981268977,1.,1.30432735639489));
#25141=CARTESIAN_POINT('Ctrl Pts',(1.54159462645432,1.,1.30630475189556));
#25142=CARTESIAN_POINT('Ctrl Pts',(1.54739413957185,1.,1.30824393907473));
#25143=CARTESIAN_POINT('Ctrl Pts',(1.55322568759481,1.,1.31014393684222));
#25144=CARTESIAN_POINT('Ctrl Pts',(1.55908521254821,1.,1.31200264341696));
#25145=CARTESIAN_POINT('Ctrl Pts',(1.56496872402353,1.,1.31381795281002));
#25146=CARTESIAN_POINT('Ctrl Pts',(1.57087397835723,1.,1.31558903860016));
#25147=CARTESIAN_POINT('Ctrl Pts',(1.5768005650559,1.,1.31731642317187));
#25148=CARTESIAN_POINT('Ctrl Pts',(1.58274907898834,1.,1.31900135021432));
#25149=CARTESIAN_POINT('Ctrl Pts',(1.58872057258245,1.,1.32064537110892));
#25150=CARTESIAN_POINT('Ctrl Pts',(1.59471591079403,1.,1.32224985747682));
#25151=CARTESIAN_POINT('Ctrl Pts',(1.60073511858687,1.,1.32381550858256));
#25152=CARTESIAN_POINT('Ctrl Pts',(1.60677758290954,1.,1.32534250785782));
#25153=CARTESIAN_POINT('Ctrl Pts',(1.6128423401575,1.,1.32683074483356));
#25154=CARTESIAN_POINT('Ctrl Pts',(1.61892832270724,1.,1.32828000610449));
#25155=CARTESIAN_POINT('Ctrl Pts',(1.62503464209797,1.,1.3296901950568));
#25156=CARTESIAN_POINT('Ctrl Pts',(1.63116079730923,1.,1.33106149345645));
#25157=CARTESIAN_POINT('Ctrl Pts',(1.63730653475089,1.,1.33239425103724));
#25158=CARTESIAN_POINT('Ctrl Pts',(1.6434717485603,1.,1.33368890676572));
#25159=CARTESIAN_POINT('Ctrl Pts',(1.6496563728683,1.,1.33494590467993));
#25160=CARTESIAN_POINT('Ctrl Pts',(1.65586025952593,1.,1.33616559745172));
#25161=CARTESIAN_POINT('Ctrl Pts',(1.66208312541983,1.,1.33734820885262));
#25162=CARTESIAN_POINT('Ctrl Pts',(1.66832460783989,1.,1.33849388654388));
#25163=CARTESIAN_POINT('Ctrl Pts',(1.67458429426086,1.,1.3396027347034));
#25164=CARTESIAN_POINT('Ctrl Pts',(1.68086176030362,1.,1.34067485185203));
#25165=CARTESIAN_POINT('Ctrl Pts',(1.68715660868764,1.,1.341710374848));
#25166=CARTESIAN_POINT('Ctrl Pts',(1.6934684849687,1.,1.34270948206319));
#25167=CARTESIAN_POINT('Ctrl Pts',(1.69979707754427,1.,1.34367237124483));
#25168=CARTESIAN_POINT('Ctrl Pts',(1.70614212266738,1.,1.34459924533831));
#25169=CARTESIAN_POINT('Ctrl Pts',(1.71250340686822,1.,1.34549029589416));
#25170=CARTESIAN_POINT('Ctrl Pts',(1.7188807715049,1.,1.34634568653227));
#25171=CARTESIAN_POINT('Ctrl Pts',(1.72527410680674,1.,1.34716554819527));
#25172=CARTESIAN_POINT('Ctrl Pts',(1.7304014965394,1.,1.34779309152035));
#25173=CARTESIAN_POINT('Ctrl Pts',(1.73425417885907,1.,1.34824783112887));
#25174=CARTESIAN_POINT('Ctrl Pts',(1.73682580585691,1.,1.34854391898045));
#25175=CARTESIAN_POINT('Ctrl Pts',(1.73811241238545,1.,1.34869019493419));
#25176=CARTESIAN_POINT('',(1.31362392696032,0.,1.15624053661742));
#25177=CARTESIAN_POINT('Origin',(0.,0.,0.));
#25178=CARTESIAN_POINT('',(1.15624053661742,1.,1.31362392696033));
#25179=CARTESIAN_POINT('Origin',(0.,1.,0.));
#25180=CARTESIAN_POINT('',(1.15624053661742,0.,1.31362392696032));
#25181=CARTESIAN_POINT('Ctrl Pts',(1.34869019493419,-1.,1.73811241238545));
#25182=CARTESIAN_POINT('Ctrl Pts',(1.34869019493419,1.,1.73811241238545));
#25183=CARTESIAN_POINT('Ctrl Pts',(1.34854391898145,-1.,1.73682580585819));
#25184=CARTESIAN_POINT('Ctrl Pts',(1.34854391898145,1.,1.73682580585819));
#25185=CARTESIAN_POINT('Ctrl Pts',(1.34824783113158,-1.,1.73425417886255));
#25186=CARTESIAN_POINT('Ctrl Pts',(1.34824783113158,1.,1.73425417886255));
#25187=CARTESIAN_POINT('Ctrl Pts',(1.3477930915247,-1.,1.73040149654497));
#25188=CARTESIAN_POINT('Ctrl Pts',(1.3477930915247,1.,1.73040149654497));
#25189=CARTESIAN_POINT('Ctrl Pts',(1.34716554820013,-1.,1.72527410681298));
#25190=CARTESIAN_POINT('Ctrl Pts',(1.34716554820013,1.,1.72527410681298));
#25191=CARTESIAN_POINT('Ctrl Pts',(1.34634568653586,-1.,1.7188807715095));
#25192=CARTESIAN_POINT('Ctrl Pts',(1.34634568653586,1.,1.7188807715095));
#25193=CARTESIAN_POINT('Ctrl Pts',(1.34549029589563,-1.,1.71250340687011));
#25194=CARTESIAN_POINT('Ctrl Pts',(1.34549029589563,1.,1.71250340687011));
#25195=CARTESIAN_POINT('Ctrl Pts',(1.34459924533783,-1.,1.70614212266676));
#25196=CARTESIAN_POINT('Ctrl Pts',(1.34459924533783,1.,1.70614212266676));
#25197=CARTESIAN_POINT('Ctrl Pts',(1.34367237124322,-1.,1.69979707754221));
#25198=CARTESIAN_POINT('Ctrl Pts',(1.34367237124322,1.,1.69979707754221));
#25199=CARTESIAN_POINT('Ctrl Pts',(1.34270948206139,-1.,1.6934684849664));
#25200=CARTESIAN_POINT('Ctrl Pts',(1.34270948206139,1.,1.6934684849664));
#25201=CARTESIAN_POINT('Ctrl Pts',(1.34171037484673,-1.,1.68715660868602));
#25202=CARTESIAN_POINT('Ctrl Pts',(1.34171037484673,1.,1.68715660868602));
#25203=CARTESIAN_POINT('Ctrl Pts',(1.3406748518516,-1.,1.68086176030308));
#25204=CARTESIAN_POINT('Ctrl Pts',(1.3406748518516,1.,1.68086176030308));
#25205=CARTESIAN_POINT('Ctrl Pts',(1.33960273470372,-1.,1.67458429426126));
#25206=CARTESIAN_POINT('Ctrl Pts',(1.33960273470372,1.,1.67458429426126));
#25207=CARTESIAN_POINT('Ctrl Pts',(1.33849388654458,-1.,1.66832460784078));
#25208=CARTESIAN_POINT('Ctrl Pts',(1.33849388654458,1.,1.66832460784078));
#25209=CARTESIAN_POINT('Ctrl Pts',(1.33734820885331,-1.,1.66208312542073));
#25210=CARTESIAN_POINT('Ctrl Pts',(1.33734820885331,1.,1.66208312542073));
#25211=CARTESIAN_POINT('Ctrl Pts',(1.33616559745217,-1.,1.65586025952651));
#25212=CARTESIAN_POINT('Ctrl Pts',(1.33616559745217,1.,1.65586025952651));
#25213=CARTESIAN_POINT('Ctrl Pts',(1.33494590468003,-1.,1.64965637286843));
#25214=CARTESIAN_POINT('Ctrl Pts',(1.33494590468003,1.,1.64965637286843));
#25215=CARTESIAN_POINT('Ctrl Pts',(1.33368890676554,-1.,1.64347174856007));
#25216=CARTESIAN_POINT('Ctrl Pts',(1.33368890676554,1.,1.64347174856007));
#25217=CARTESIAN_POINT('Ctrl Pts',(1.33239425103694,-1.,1.6373065347505));
#25218=CARTESIAN_POINT('Ctrl Pts',(1.33239425103694,1.,1.6373065347505));
#25219=CARTESIAN_POINT('Ctrl Pts',(1.33106149345618,-1.,1.63116079730887));
#25220=CARTESIAN_POINT('Ctrl Pts',(1.33106149345618,1.,1.63116079730887));
#25221=CARTESIAN_POINT('Ctrl Pts',(1.32969019505665,-1.,1.62503464209777));
#25222=CARTESIAN_POINT('Ctrl Pts',(1.32969019505665,1.,1.62503464209777));
#25223=CARTESIAN_POINT('Ctrl Pts',(1.32828000610448,-1.,1.61892832270723));
#25224=CARTESIAN_POINT('Ctrl Pts',(1.32828000610448,1.,1.61892832270723));
#25225=CARTESIAN_POINT('Ctrl Pts',(1.32683074483365,-1.,1.61284234015762));
#25226=CARTESIAN_POINT('Ctrl Pts',(1.32683074483365,1.,1.61284234015762));
#25227=CARTESIAN_POINT('Ctrl Pts',(1.32534250785794,-1.,1.6067775829097));
#25228=CARTESIAN_POINT('Ctrl Pts',(1.32534250785794,1.,1.6067775829097));
#25229=CARTESIAN_POINT('Ctrl Pts',(1.32381550858266,-1.,1.600735118587));
#25230=CARTESIAN_POINT('Ctrl Pts',(1.32381550858266,1.,1.600735118587));
#25231=CARTESIAN_POINT('Ctrl Pts',(1.32224985747686,-1.,1.59471591079408));
#25232=CARTESIAN_POINT('Ctrl Pts',(1.32224985747686,1.,1.59471591079408));
#25233=CARTESIAN_POINT('Ctrl Pts',(1.32064537110891,-1.,1.58872057258244));
#25234=CARTESIAN_POINT('Ctrl Pts',(1.32064537110891,1.,1.58872057258244));
#25235=CARTESIAN_POINT('Ctrl Pts',(1.31900135021428,-1.,1.58274907898829));
#25236=CARTESIAN_POINT('Ctrl Pts',(1.31900135021428,1.,1.58274907898829));
#25237=CARTESIAN_POINT('Ctrl Pts',(1.31731642317183,-1.,1.57680056505585));
#25238=CARTESIAN_POINT('Ctrl Pts',(1.31731642317183,1.,1.57680056505585));
#25239=CARTESIAN_POINT('Ctrl Pts',(1.31558903860015,-1.,1.57087397835721));
#25240=CARTESIAN_POINT('Ctrl Pts',(1.31558903860015,1.,1.57087397835721));
#25241=CARTESIAN_POINT('Ctrl Pts',(1.31381795281002,-1.,1.56496872402352));
#25242=CARTESIAN_POINT('Ctrl Pts',(1.31381795281002,1.,1.56496872402352));
#25243=CARTESIAN_POINT('Ctrl Pts',(1.31200264341696,-1.,1.55908521254822));
#25244=CARTESIAN_POINT('Ctrl Pts',(1.31200264341696,1.,1.55908521254822));
#25245=CARTESIAN_POINT('Ctrl Pts',(1.31014393684221,-1.,1.55322568759481));
#25246=CARTESIAN_POINT('Ctrl Pts',(1.31014393684221,1.,1.55322568759481));
#25247=CARTESIAN_POINT('Ctrl Pts',(1.30824393907471,-1.,1.54739413957183));
#25248=CARTESIAN_POINT('Ctrl Pts',(1.30824393907471,1.,1.54739413957183));
#25249=CARTESIAN_POINT('Ctrl Pts',(1.30630475189553,-1.,1.54159462645428));
#25250=CARTESIAN_POINT('Ctrl Pts',(1.30630475189553,1.,1.54159462645428));
#25251=CARTESIAN_POINT('Ctrl Pts',(1.30432735639487,-1.,1.53582981268976));
#25252=CARTESIAN_POINT('Ctrl Pts',(1.30432735639487,1.,1.53582981268976));
#25253=CARTESIAN_POINT('Ctrl Pts',(1.3023106439557,-1.,1.53009970283893));
#25254=CARTESIAN_POINT('Ctrl Pts',(1.3023106439557,1.,1.53009970283893));
#25255=CARTESIAN_POINT('Ctrl Pts',(1.30024984366334,-1.,1.5243995786107));
#25256=CARTESIAN_POINT('Ctrl Pts',(1.30024984366334,1.,1.5243995786107));
#25257=CARTESIAN_POINT('Ctrl Pts',(1.29813791800757,-1.,1.51872184912735));
#25258=CARTESIAN_POINT('Ctrl Pts',(1.29813791800757,1.,1.51872184912735));
#25259=CARTESIAN_POINT('Ctrl Pts',(1.29596850710518,-1.,1.51305994241412));
#25260=CARTESIAN_POINT('Ctrl Pts',(1.29596850710518,1.,1.51305994241412));
#25261=CARTESIAN_POINT('Ctrl Pts',(1.29373841372843,-1.,1.50741159078367));
#25262=CARTESIAN_POINT('Ctrl Pts',(1.29373841372843,1.,1.50741159078367));
#25263=CARTESIAN_POINT('Ctrl Pts',(1.29145022885171,-1.,1.50178230149764));
#25264=CARTESIAN_POINT('Ctrl Pts',(1.29145022885171,1.,1.50178230149764));
#25265=CARTESIAN_POINT('Ctrl Pts',(1.28911506584232,-1.,1.49618896881729));
#25266=CARTESIAN_POINT('Ctrl Pts',(1.28911506584232,1.,1.49618896881729));
#25267=CARTESIAN_POINT('Ctrl Pts',(1.28674676116415,-1.,1.4906522831275));
#25268=CARTESIAN_POINT('Ctrl Pts',(1.28674676116415,1.,1.4906522831275));
#25269=CARTESIAN_POINT('Ctrl Pts',(1.28435533880184,-1.,1.48518817118891));
#25270=CARTESIAN_POINT('Ctrl Pts',(1.28435533880184,1.,1.48518817118891));
#25271=CARTESIAN_POINT('Ctrl Pts',(1.28194158939522,-1.,1.47980070347102));
#25272=CARTESIAN_POINT('Ctrl Pts',(1.28194158939522,1.,1.47980070347102));
#25273=CARTESIAN_POINT('Ctrl Pts',(1.27948918248524,-1.,1.4744717526711));
#25274=CARTESIAN_POINT('Ctrl Pts',(1.27948918248524,1.,1.4744717526711));
#25275=CARTESIAN_POINT('Ctrl Pts',(1.27696414831144,-1.,1.46916035917197));
#25276=CARTESIAN_POINT('Ctrl Pts',(1.27696414831144,1.,1.46916035917197));
#25277=CARTESIAN_POINT('Ctrl Pts',(1.27433119897877,-1.,1.4638243133254));
#25278=CARTESIAN_POINT('Ctrl Pts',(1.27433119897877,1.,1.4638243133254));
#25279=CARTESIAN_POINT('Ctrl Pts',(1.27156805265312,-1.,1.45843906294725));
#25280=CARTESIAN_POINT('Ctrl Pts',(1.27156805265312,1.,1.45843906294725));
#25281=CARTESIAN_POINT('Ctrl Pts',(1.26867786804854,-1.,1.45301422764205));
#25282=CARTESIAN_POINT('Ctrl Pts',(1.26867786804854,1.,1.45301422764205));
#25283=CARTESIAN_POINT('Ctrl Pts',(1.26570925118767,-1.,1.44761985001544));
#25284=CARTESIAN_POINT('Ctrl Pts',(1.26570925118767,1.,1.44761985001544));
#25285=CARTESIAN_POINT('Ctrl Pts',(1.26273903323723,-1.,1.44236470511145));
#25286=CARTESIAN_POINT('Ctrl Pts',(1.26273903323723,1.,1.44236470511145));
#25287=CARTESIAN_POINT('Ctrl Pts',(1.25983531011894,-1.,1.43734919180719));
#25288=CARTESIAN_POINT('Ctrl Pts',(1.25983531011894,1.,1.43734919180719));
#25289=CARTESIAN_POINT('Ctrl Pts',(1.25702687965744,-1.,1.43262645609679));
#25290=CARTESIAN_POINT('Ctrl Pts',(1.25702687965744,1.,1.43262645609679));
#25291=CARTESIAN_POINT('Ctrl Pts',(1.25426945222783,-1.,1.42815938799555));
#25292=CARTESIAN_POINT('Ctrl Pts',(1.25426945222783,1.,1.42815938799555));
#25293=CARTESIAN_POINT('Ctrl Pts',(1.25141455570299,-1.,1.42378102115911));
#25294=CARTESIAN_POINT('Ctrl Pts',(1.25141455570299,1.,1.42378102115911));
#25295=CARTESIAN_POINT('Ctrl Pts',(1.24824430986911,-1.,1.41923722596421));
#25296=CARTESIAN_POINT('Ctrl Pts',(1.24824430986911,1.,1.41923722596421));
#25297=CARTESIAN_POINT('Ctrl Pts',(1.24450600513278,-1.,1.41422913175437));
#25298=CARTESIAN_POINT('Ctrl Pts',(1.24450600513278,1.,1.41422913175437));
#25299=CARTESIAN_POINT('Ctrl Pts',(1.23994455029421,-1.,1.40845295531151));
#25300=CARTESIAN_POINT('Ctrl Pts',(1.23994455029421,1.,1.40845295531151));
#25301=CARTESIAN_POINT('Ctrl Pts',(1.23434087289768,-1.,1.40164708205345));
#25302=CARTESIAN_POINT('Ctrl Pts',(1.23434087289768,1.,1.40164708205345));
#25303=CARTESIAN_POINT('Ctrl Pts',(1.22752961898063,-1.,1.39361389567257));
#25304=CARTESIAN_POINT('Ctrl Pts',(1.22752961898063,1.,1.39361389567257));
#25305=CARTESIAN_POINT('Ctrl Pts',(1.21938737278853,-1.,1.38420564525391));
#25306=CARTESIAN_POINT('Ctrl Pts',(1.21938737278853,1.,1.38420564525391));
#25307=CARTESIAN_POINT('Ctrl Pts',(1.20982812923113,-1.,1.37331915604962));
#25308=CARTESIAN_POINT('Ctrl Pts',(1.20982812923113,1.,1.37331915604962));
#25309=CARTESIAN_POINT('Ctrl Pts',(1.1987959077656,-1.,1.36088705040677));
#25310=CARTESIAN_POINT('Ctrl Pts',(1.1987959077656,1.,1.36088705040677));
#25311=CARTESIAN_POINT('Ctrl Pts',(1.18625865664915,-1.,1.34687053998157));
#25312=CARTESIAN_POINT('Ctrl Pts',(1.18625865664915,1.,1.34687053998157));
#25313=CARTESIAN_POINT('Ctrl Pts',(1.17501305787994,-1.,1.33437539344842));
#25314=CARTESIAN_POINT('Ctrl Pts',(1.17501305787994,1.,1.33437539344842));
#25315=CARTESIAN_POINT('Ctrl Pts',(1.16589330092532,-1.,1.32428080720544));
#25316=CARTESIAN_POINT('Ctrl Pts',(1.16589330092532,1.,1.32428080720544));
#25317=CARTESIAN_POINT('Ctrl Pts',(1.15950888730433,-1.,1.3172297721596));
#25318=CARTESIAN_POINT('Ctrl Pts',(1.15950888730433,1.,1.3172297721596));
#25319=CARTESIAN_POINT('Ctrl Pts',(1.15624053661742,-1.,1.31362392696033));
#25320=CARTESIAN_POINT('Ctrl Pts',(1.15624053661742,1.,1.31362392696033));
#25321=CARTESIAN_POINT('',(1.34869019493419,1.,1.73811241238545));
#25322=CARTESIAN_POINT('Ctrl Pts',(1.34869019493419,1.,1.73811241238545));
#25323=CARTESIAN_POINT('Ctrl Pts',(1.34854391898145,1.,1.73682580585819));
#25324=CARTESIAN_POINT('Ctrl Pts',(1.34824783113158,1.,1.73425417886255));
#25325=CARTESIAN_POINT('Ctrl Pts',(1.3477930915247,1.,1.73040149654497));
#25326=CARTESIAN_POINT('Ctrl Pts',(1.34716554820013,1.,1.72527410681298));
#25327=CARTESIAN_POINT('Ctrl Pts',(1.34634568653586,1.,1.7188807715095));
#25328=CARTESIAN_POINT('Ctrl Pts',(1.34549029589563,1.,1.71250340687011));
#25329=CARTESIAN_POINT('Ctrl Pts',(1.34459924533783,1.,1.70614212266676));
#25330=CARTESIAN_POINT('Ctrl Pts',(1.34367237124322,1.,1.69979707754221));
#25331=CARTESIAN_POINT('Ctrl Pts',(1.34270948206139,1.,1.6934684849664));
#25332=CARTESIAN_POINT('Ctrl Pts',(1.34171037484673,1.,1.68715660868602));
#25333=CARTESIAN_POINT('Ctrl Pts',(1.3406748518516,1.,1.68086176030308));
#25334=CARTESIAN_POINT('Ctrl Pts',(1.33960273470372,1.,1.67458429426126));
#25335=CARTESIAN_POINT('Ctrl Pts',(1.33849388654458,1.,1.66832460784078));
#25336=CARTESIAN_POINT('Ctrl Pts',(1.33734820885331,1.,1.66208312542073));
#25337=CARTESIAN_POINT('Ctrl Pts',(1.33616559745217,1.,1.65586025952651));
#25338=CARTESIAN_POINT('Ctrl Pts',(1.33494590468003,1.,1.64965637286843));
#25339=CARTESIAN_POINT('Ctrl Pts',(1.33368890676554,1.,1.64347174856007));
#25340=CARTESIAN_POINT('Ctrl Pts',(1.33239425103694,1.,1.6373065347505));
#25341=CARTESIAN_POINT('Ctrl Pts',(1.33106149345618,1.,1.63116079730887));
#25342=CARTESIAN_POINT('Ctrl Pts',(1.32969019505665,1.,1.62503464209777));
#25343=CARTESIAN_POINT('Ctrl Pts',(1.32828000610448,1.,1.61892832270723));
#25344=CARTESIAN_POINT('Ctrl Pts',(1.32683074483365,1.,1.61284234015762));
#25345=CARTESIAN_POINT('Ctrl Pts',(1.32534250785794,1.,1.6067775829097));
#25346=CARTESIAN_POINT('Ctrl Pts',(1.32381550858266,1.,1.600735118587));
#25347=CARTESIAN_POINT('Ctrl Pts',(1.32224985747686,1.,1.59471591079408));
#25348=CARTESIAN_POINT('Ctrl Pts',(1.32064537110891,1.,1.58872057258244));
#25349=CARTESIAN_POINT('Ctrl Pts',(1.31900135021428,1.,1.58274907898829));
#25350=CARTESIAN_POINT('Ctrl Pts',(1.31731642317183,1.,1.57680056505585));
#25351=CARTESIAN_POINT('Ctrl Pts',(1.31558903860015,1.,1.57087397835721));
#25352=CARTESIAN_POINT('Ctrl Pts',(1.31381795281002,1.,1.56496872402352));
#25353=CARTESIAN_POINT('Ctrl Pts',(1.31200264341696,1.,1.55908521254822));
#25354=CARTESIAN_POINT('Ctrl Pts',(1.31014393684221,1.,1.55322568759481));
#25355=CARTESIAN_POINT('Ctrl Pts',(1.30824393907471,1.,1.54739413957183));
#25356=CARTESIAN_POINT('Ctrl Pts',(1.30630475189553,1.,1.54159462645428));
#25357=CARTESIAN_POINT('Ctrl Pts',(1.30432735639487,1.,1.53582981268976));
#25358=CARTESIAN_POINT('Ctrl Pts',(1.3023106439557,1.,1.53009970283893));
#25359=CARTESIAN_POINT('Ctrl Pts',(1.30024984366334,1.,1.5243995786107));
#25360=CARTESIAN_POINT('Ctrl Pts',(1.29813791800757,1.,1.51872184912735));
#25361=CARTESIAN_POINT('Ctrl Pts',(1.29596850710518,1.,1.51305994241412));
#25362=CARTESIAN_POINT('Ctrl Pts',(1.29373841372843,1.,1.50741159078367));
#25363=CARTESIAN_POINT('Ctrl Pts',(1.29145022885171,1.,1.50178230149764));
#25364=CARTESIAN_POINT('Ctrl Pts',(1.28911506584232,1.,1.49618896881729));
#25365=CARTESIAN_POINT('Ctrl Pts',(1.28674676116415,1.,1.4906522831275));
#25366=CARTESIAN_POINT('Ctrl Pts',(1.28435533880184,1.,1.48518817118891));
#25367=CARTESIAN_POINT('Ctrl Pts',(1.28194158939522,1.,1.47980070347102));
#25368=CARTESIAN_POINT('Ctrl Pts',(1.27948918248524,1.,1.4744717526711));
#25369=CARTESIAN_POINT('Ctrl Pts',(1.27696414831144,1.,1.46916035917197));
#25370=CARTESIAN_POINT('Ctrl Pts',(1.27433119897877,1.,1.4638243133254));
#25371=CARTESIAN_POINT('Ctrl Pts',(1.27156805265312,1.,1.45843906294725));
#25372=CARTESIAN_POINT('Ctrl Pts',(1.26867786804854,1.,1.45301422764205));
#25373=CARTESIAN_POINT('Ctrl Pts',(1.26570925118767,1.,1.44761985001544));
#25374=CARTESIAN_POINT('Ctrl Pts',(1.26273903323723,1.,1.44236470511145));
#25375=CARTESIAN_POINT('Ctrl Pts',(1.25983531011894,1.,1.43734919180719));
#25376=CARTESIAN_POINT('Ctrl Pts',(1.25702687965744,1.,1.43262645609679));
#25377=CARTESIAN_POINT('Ctrl Pts',(1.25426945222783,1.,1.42815938799555));
#25378=CARTESIAN_POINT('Ctrl Pts',(1.25141455570299,1.,1.42378102115911));
#25379=CARTESIAN_POINT('Ctrl Pts',(1.24824430986911,1.,1.41923722596421));
#25380=CARTESIAN_POINT('Ctrl Pts',(1.24450600513278,1.,1.41422913175437));
#25381=CARTESIAN_POINT('Ctrl Pts',(1.23994455029421,1.,1.40845295531151));
#25382=CARTESIAN_POINT('Ctrl Pts',(1.23434087289768,1.,1.40164708205345));
#25383=CARTESIAN_POINT('Ctrl Pts',(1.22752961898063,1.,1.39361389567257));
#25384=CARTESIAN_POINT('Ctrl Pts',(1.21938737278853,1.,1.38420564525391));
#25385=CARTESIAN_POINT('Ctrl Pts',(1.20982812923113,1.,1.37331915604962));
#25386=CARTESIAN_POINT('Ctrl Pts',(1.1987959077656,1.,1.36088705040677));
#25387=CARTESIAN_POINT('Ctrl Pts',(1.18625865664915,1.,1.34687053998157));
#25388=CARTESIAN_POINT('Ctrl Pts',(1.17501305787994,1.,1.33437539344842));
#25389=CARTESIAN_POINT('Ctrl Pts',(1.16589330092532,1.,1.32428080720544));
#25390=CARTESIAN_POINT('Ctrl Pts',(1.15950888730433,1.,1.3172297721596));
#25391=CARTESIAN_POINT('Ctrl Pts',(1.15624053661742,1.,1.31362392696033));
#25392=CARTESIAN_POINT('',(1.34869019493419,0.,1.73811241238545));
#25393=CARTESIAN_POINT('Origin',(1.23627494547115,0.,1.81978687191668));
#25394=CARTESIAN_POINT('',(1.23627494547115,1.,1.81978687191668));
#25395=CARTESIAN_POINT('',(1.34869019493419,1.,1.73811241238545));
#25396=CARTESIAN_POINT('',(1.23627494547115,0.,1.81978687191668));
#25397=CARTESIAN_POINT('Ctrl Pts',(0.892032620296855,-1.,1.5055822144029));
#25398=CARTESIAN_POINT('Ctrl Pts',(0.892032620296855,1.,1.5055822144029));
#25399=CARTESIAN_POINT('Ctrl Pts',(0.894452006967538,-1.,1.50980486807181));
#25400=CARTESIAN_POINT('Ctrl Pts',(0.894452006967538,1.,1.50980486807181));
#25401=CARTESIAN_POINT('Ctrl Pts',(0.89918504749193,-1.,1.51805569591479));
#25402=CARTESIAN_POINT('Ctrl Pts',(0.89918504749193,1.,1.51805569591479));
#25403=CARTESIAN_POINT('Ctrl Pts',(0.905967409640498,-1.,1.52984849890434));
#25404=CARTESIAN_POINT('Ctrl Pts',(0.905967409640498,1.,1.52984849890434));
#25405=CARTESIAN_POINT('Ctrl Pts',(0.914375919046579,-1.,1.54440491152808));
#25406=CARTESIAN_POINT('Ctrl Pts',(0.914375919046579,1.,1.54440491152808));
#25407=CARTESIAN_POINT('Ctrl Pts',(0.923832188966322,-1.,1.56065988582509));
#25408=CARTESIAN_POINT('Ctrl Pts',(0.923832188966322,1.,1.56065988582509));
#25409=CARTESIAN_POINT('Ctrl Pts',(0.932246680128848,-1.,1.57499388385561));
#25410=CARTESIAN_POINT('Ctrl Pts',(0.932246680128848,1.,1.57499388385561));
#25411=CARTESIAN_POINT('Ctrl Pts',(0.939646377909319,-1.,1.58744937489796));
#25412=CARTESIAN_POINT('Ctrl Pts',(0.939646377909319,1.,1.58744937489796));
#25413=CARTESIAN_POINT('Ctrl Pts',(0.946078063325795,-1.,1.59810042045408));
#25414=CARTESIAN_POINT('Ctrl Pts',(0.946078063325795,1.,1.59810042045408));
#25415=CARTESIAN_POINT('Ctrl Pts',(0.951613284361247,-1.,1.60706069897794));
#25416=CARTESIAN_POINT('Ctrl Pts',(0.951613284361247,1.,1.60706069897794));
#25417=CARTESIAN_POINT('Ctrl Pts',(0.956354422921572,-1.,1.61449324337233));
#25418=CARTESIAN_POINT('Ctrl Pts',(0.956354422921572,1.,1.61449324337233));
#25419=CARTESIAN_POINT('Ctrl Pts',(0.960438326099958,-1.,1.62061638139929));
#25420=CARTESIAN_POINT('Ctrl Pts',(0.960438326099958,1.,1.62061638139929));
#25421=CARTESIAN_POINT('Ctrl Pts',(0.964046107037821,-1.,1.6257193066974));
#25422=CARTESIAN_POINT('Ctrl Pts',(0.964046107037821,1.,1.6257193066974));
#25423=CARTESIAN_POINT('Ctrl Pts',(0.967387853228041,-1.,1.63013849959083));
#25424=CARTESIAN_POINT('Ctrl Pts',(0.967387853228041,1.,1.63013849959083));
#25425=CARTESIAN_POINT('Ctrl Pts',(0.970669715996356,-1.,1.63420665729609));
#25426=CARTESIAN_POINT('Ctrl Pts',(0.970669715996356,1.,1.63420665729609));
#25427=CARTESIAN_POINT('Ctrl Pts',(0.974066058287501,-1.,1.63820952658157));
#25428=CARTESIAN_POINT('Ctrl Pts',(0.974066058287501,1.,1.63820952658157));
#25429=CARTESIAN_POINT('Ctrl Pts',(0.977689794120296,-1.,1.64233990826831));
#25430=CARTESIAN_POINT('Ctrl Pts',(0.977689794120296,1.,1.64233990826831));
#25431=CARTESIAN_POINT('Ctrl Pts',(0.981562530940574,-1.,1.64665139190834));
#25432=CARTESIAN_POINT('Ctrl Pts',(0.981562530940574,1.,1.64665139190834));
#25433=CARTESIAN_POINT('Ctrl Pts',(0.985642622921626,-1.,1.6511001661277));
#25434=CARTESIAN_POINT('Ctrl Pts',(0.985642622921626,1.,1.6511001661277));
#25435=CARTESIAN_POINT('Ctrl Pts',(0.98985562785445,-1.,1.65559044289746));
#25436=CARTESIAN_POINT('Ctrl Pts',(0.98985562785445,1.,1.65559044289746));
#25437=CARTESIAN_POINT('Ctrl Pts',(0.994121836661115,-1.,1.66001553809916));
#25438=CARTESIAN_POINT('Ctrl Pts',(0.994121836661115,1.,1.66001553809916));
#25439=CARTESIAN_POINT('Ctrl Pts',(0.998389654952317,-1.,1.66430758030304));
#25440=CARTESIAN_POINT('Ctrl Pts',(0.998389654952317,1.,1.66430758030304));
#25441=CARTESIAN_POINT('Ctrl Pts',(1.00265091003682,-1.,1.66846059277231));
#25442=CARTESIAN_POINT('Ctrl Pts',(1.00265091003682,1.,1.66846059277231));
#25443=CARTESIAN_POINT('Ctrl Pts',(1.00692206696387,-1.,1.67250335383248));
#25444=CARTESIAN_POINT('Ctrl Pts',(1.00692206696387,1.,1.67250335383248));
#25445=CARTESIAN_POINT('Ctrl Pts',(1.01123236493507,-1.,1.67648246776457));
#25446=CARTESIAN_POINT('Ctrl Pts',(1.01123236493507,1.,1.67648246776457));
#25447=CARTESIAN_POINT('Ctrl Pts',(1.01561026162786,-1.,1.6804428989482));
#25448=CARTESIAN_POINT('Ctrl Pts',(1.01561026162786,1.,1.6804428989482));
#25449=CARTESIAN_POINT('Ctrl Pts',(1.02006795074222,-1.,1.68440578021739));
#25450=CARTESIAN_POINT('Ctrl Pts',(1.02006795074222,1.,1.68440578021739));
#25451=CARTESIAN_POINT('Ctrl Pts',(1.02460180535272,-1.,1.68836910178475));
#25452=CARTESIAN_POINT('Ctrl Pts',(1.02460180535272,1.,1.68836910178475));
#25453=CARTESIAN_POINT('Ctrl Pts',(1.02919977579155,-1.,1.69231840863471));
#25454=CARTESIAN_POINT('Ctrl Pts',(1.02919977579155,1.,1.69231840863471));
#25455=CARTESIAN_POINT('Ctrl Pts',(1.03384646003587,-1.,1.69623414782769));
#25456=CARTESIAN_POINT('Ctrl Pts',(1.03384646003587,1.,1.69623414782769));
#25457=CARTESIAN_POINT('Ctrl Pts',(1.03852922490782,-1.,1.70010052930951));
#25458=CARTESIAN_POINT('Ctrl Pts',(1.03852922490782,1.,1.70010052930951));
#25459=CARTESIAN_POINT('Ctrl Pts',(1.04324363334546,-1.,1.70391338707969));
#25460=CARTESIAN_POINT('Ctrl Pts',(1.04324363334546,1.,1.70391338707969));
#25461=CARTESIAN_POINT('Ctrl Pts',(1.0479908540499,-1.,1.70767646263641));
#25462=CARTESIAN_POINT('Ctrl Pts',(1.0479908540499,1.,1.70767646263641));
#25463=CARTESIAN_POINT('Ctrl Pts',(1.05277517202853,-1.,1.71139783543986));
#25464=CARTESIAN_POINT('Ctrl Pts',(1.05277517202853,1.,1.71139783543986));
#25465=CARTESIAN_POINT('Ctrl Pts',(1.05760163192481,-1.,1.71508654427022));
#25466=CARTESIAN_POINT('Ctrl Pts',(1.05760163192481,1.,1.71508654427022));
#25467=CARTESIAN_POINT('Ctrl Pts',(1.06247324680649,-1.,1.71874858456908));
#25468=CARTESIAN_POINT('Ctrl Pts',(1.06247324680649,1.,1.71874858456908));
#25469=CARTESIAN_POINT('Ctrl Pts',(1.06738966975463,-1.,1.72238500928456));
#25470=CARTESIAN_POINT('Ctrl Pts',(1.06738966975463,1.,1.72238500928456));
#25471=CARTESIAN_POINT('Ctrl Pts',(1.07234866990252,-1.,1.72599406198489));
#25472=CARTESIAN_POINT('Ctrl Pts',(1.07234866990252,1.,1.72599406198489));
#25473=CARTESIAN_POINT('Ctrl Pts',(1.0773470373727,-1.,1.72957248977424));
#25474=CARTESIAN_POINT('Ctrl Pts',(1.0773470373727,1.,1.72957248977424));
#25475=CARTESIAN_POINT('Ctrl Pts',(1.08238162784749,-1.,1.73311705663407));
#25476=CARTESIAN_POINT('Ctrl Pts',(1.08238162784749,1.,1.73311705663407));
#25477=CARTESIAN_POINT('Ctrl Pts',(1.08745056285429,-1.,1.73662628326093));
#25478=CARTESIAN_POINT('Ctrl Pts',(1.08745056285429,1.,1.73662628326093));
#25479=CARTESIAN_POINT('Ctrl Pts',(1.09255329056496,-1.,1.74010053962252));
#25480=CARTESIAN_POINT('Ctrl Pts',(1.09255329056496,1.,1.74010053962252));
#25481=CARTESIAN_POINT('Ctrl Pts',(1.09768999241229,-1.,1.74354119236212));
#25482=CARTESIAN_POINT('Ctrl Pts',(1.09768999241229,1.,1.74354119236212));
#25483=CARTESIAN_POINT('Ctrl Pts',(1.10286118991144,-1.,1.74695004214924));
#25484=CARTESIAN_POINT('Ctrl Pts',(1.10286118991144,1.,1.74695004214924));
#25485=CARTESIAN_POINT('Ctrl Pts',(1.10806728183003,-1.,1.75032866075914));
#25486=CARTESIAN_POINT('Ctrl Pts',(1.10806728183003,1.,1.75032866075914));
#25487=CARTESIAN_POINT('Ctrl Pts',(1.11330807582542,-1.,1.75367772094617));
#25488=CARTESIAN_POINT('Ctrl Pts',(1.11330807582542,1.,1.75367772094617));
#25489=CARTESIAN_POINT('Ctrl Pts',(1.11858293216752,-1.,1.75699720772089));
#25490=CARTESIAN_POINT('Ctrl Pts',(1.11858293216752,1.,1.75699720772089));
#25491=CARTESIAN_POINT('Ctrl Pts',(1.12389096855078,-1.,1.76028671825084));
#25492=CARTESIAN_POINT('Ctrl Pts',(1.12389096855078,1.,1.76028671825084));
#25493=CARTESIAN_POINT('Ctrl Pts',(1.12923123555076,-1.,1.76354571966171));
#25494=CARTESIAN_POINT('Ctrl Pts',(1.12923123555076,1.,1.76354571966171));
#25495=CARTESIAN_POINT('Ctrl Pts',(1.13460291804634,-1.,1.76677384551883));
#25496=CARTESIAN_POINT('Ctrl Pts',(1.13460291804634,1.,1.76677384551883));
#25497=CARTESIAN_POINT('Ctrl Pts',(1.14000548337,-1.,1.76997111386806));
#25498=CARTESIAN_POINT('Ctrl Pts',(1.14000548337,1.,1.76997111386806));
#25499=CARTESIAN_POINT('Ctrl Pts',(1.14543858226948,-1.,1.77313777896234));
#25500=CARTESIAN_POINT('Ctrl Pts',(1.14543858226948,1.,1.77313777896234));
#25501=CARTESIAN_POINT('Ctrl Pts',(1.15090197841531,-1.,1.77627422557034));
#25502=CARTESIAN_POINT('Ctrl Pts',(1.15090197841531,1.,1.77627422557034));
#25503=CARTESIAN_POINT('Ctrl Pts',(1.15639547194689,-1.,1.77938085564261));
#25504=CARTESIAN_POINT('Ctrl Pts',(1.15639547194689,1.,1.77938085564261));
#25505=CARTESIAN_POINT('Ctrl Pts',(1.16191881298458,-1.,1.78245795880949));
#25506=CARTESIAN_POINT('Ctrl Pts',(1.16191881298458,1.,1.78245795880949));
#25507=CARTESIAN_POINT('Ctrl Pts',(1.16747166312239,-1.,1.78550566040349));
#25508=CARTESIAN_POINT('Ctrl Pts',(1.16747166312239,1.,1.78550566040349));
#25509=CARTESIAN_POINT('Ctrl Pts',(1.17305363177265,-1.,1.78852398877523));
#25510=CARTESIAN_POINT('Ctrl Pts',(1.17305363177265,1.,1.78852398877523));
#25511=CARTESIAN_POINT('Ctrl Pts',(1.17866429440781,-1.,1.79151291552646));
#25512=CARTESIAN_POINT('Ctrl Pts',(1.17866429440781,1.,1.79151291552646));
#25513=CARTESIAN_POINT('Ctrl Pts',(1.18430321697471,-1.,1.79447240321572));
#25514=CARTESIAN_POINT('Ctrl Pts',(1.18430321697471,1.,1.79447240321572));
#25515=CARTESIAN_POINT('Ctrl Pts',(1.1899699793456,-1.,1.79740245923649));
#25516=CARTESIAN_POINT('Ctrl Pts',(1.1899699793456,1.,1.79740245923649));
#25517=CARTESIAN_POINT('Ctrl Pts',(1.19566418930405,-1.,1.80030314370121));
#25518=CARTESIAN_POINT('Ctrl Pts',(1.19566418930405,1.,1.80030314370121));
#25519=CARTESIAN_POINT('Ctrl Pts',(1.2013854893912,-1.,1.8031745483882));
#25520=CARTESIAN_POINT('Ctrl Pts',(1.2013854893912,1.,1.8031745483882));
#25521=CARTESIAN_POINT('Ctrl Pts',(1.20713356605519,-1.,1.80601678480772));
#25522=CARTESIAN_POINT('Ctrl Pts',(1.20713356605519,1.,1.80601678480772));
#25523=CARTESIAN_POINT('Ctrl Pts',(1.2129081570818,-1.,1.80882996916931));
#25524=CARTESIAN_POINT('Ctrl Pts',(1.2129081570818,1.,1.80882996916931));
#25525=CARTESIAN_POINT('Ctrl Pts',(1.2187090610323,-1.,1.81161420806172));
#25526=CARTESIAN_POINT('Ctrl Pts',(1.2187090610323,1.,1.81161420806172));
#25527=CARTESIAN_POINT('Ctrl Pts',(1.22453613304507,-1.,1.81436959209778));
#25528=CARTESIAN_POINT('Ctrl Pts',(1.22453613304507,1.,1.81436959209778));
#25529=CARTESIAN_POINT('Ctrl Pts',(1.22921864890975,-1.,1.81655087183054));
#25530=CARTESIAN_POINT('Ctrl Pts',(1.22921864890975,1.,1.81655087183054));
#25531=CARTESIAN_POINT('Ctrl Pts',(1.23274224526804,-1.,1.81817389920914));
#25532=CARTESIAN_POINT('Ctrl Pts',(1.23274224526804,1.,1.81817389920914));
#25533=CARTESIAN_POINT('Ctrl Pts',(1.23509651170384,-1.,1.81925017193531));
#25534=CARTESIAN_POINT('Ctrl Pts',(1.23509651170384,1.,1.81925017193531));
#25535=CARTESIAN_POINT('Ctrl Pts',(1.23627494547115,-1.,1.81978687191668));
#25536=CARTESIAN_POINT('Ctrl Pts',(1.23627494547115,1.,1.81978687191668));
#25537=CARTESIAN_POINT('',(0.892032620296855,1.,1.5055822144029));
#25538=CARTESIAN_POINT('Ctrl Pts',(0.892032620296855,1.,1.5055822144029));
#25539=CARTESIAN_POINT('Ctrl Pts',(0.894452006967538,1.,1.50980486807181));
#25540=CARTESIAN_POINT('Ctrl Pts',(0.89918504749193,1.,1.51805569591479));
#25541=CARTESIAN_POINT('Ctrl Pts',(0.905967409640498,1.,1.52984849890434));
#25542=CARTESIAN_POINT('Ctrl Pts',(0.914375919046579,1.,1.54440491152808));
#25543=CARTESIAN_POINT('Ctrl Pts',(0.923832188966322,1.,1.56065988582509));
#25544=CARTESIAN_POINT('Ctrl Pts',(0.932246680128848,1.,1.57499388385561));
#25545=CARTESIAN_POINT('Ctrl Pts',(0.939646377909319,1.,1.58744937489796));
#25546=CARTESIAN_POINT('Ctrl Pts',(0.946078063325795,1.,1.59810042045408));
#25547=CARTESIAN_POINT('Ctrl Pts',(0.951613284361247,1.,1.60706069897794));
#25548=CARTESIAN_POINT('Ctrl Pts',(0.956354422921572,1.,1.61449324337233));
#25549=CARTESIAN_POINT('Ctrl Pts',(0.960438326099958,1.,1.62061638139929));
#25550=CARTESIAN_POINT('Ctrl Pts',(0.964046107037821,1.,1.6257193066974));
#25551=CARTESIAN_POINT('Ctrl Pts',(0.967387853228041,1.,1.63013849959083));
#25552=CARTESIAN_POINT('Ctrl Pts',(0.970669715996356,1.,1.63420665729609));
#25553=CARTESIAN_POINT('Ctrl Pts',(0.974066058287501,1.,1.63820952658157));
#25554=CARTESIAN_POINT('Ctrl Pts',(0.977689794120296,1.,1.64233990826831));
#25555=CARTESIAN_POINT('Ctrl Pts',(0.981562530940574,1.,1.64665139190834));
#25556=CARTESIAN_POINT('Ctrl Pts',(0.985642622921626,1.,1.6511001661277));
#25557=CARTESIAN_POINT('Ctrl Pts',(0.98985562785445,1.,1.65559044289746));
#25558=CARTESIAN_POINT('Ctrl Pts',(0.994121836661115,1.,1.66001553809916));
#25559=CARTESIAN_POINT('Ctrl Pts',(0.998389654952317,1.,1.66430758030304));
#25560=CARTESIAN_POINT('Ctrl Pts',(1.00265091003682,1.,1.66846059277231));
#25561=CARTESIAN_POINT('Ctrl Pts',(1.00692206696387,1.,1.67250335383248));
#25562=CARTESIAN_POINT('Ctrl Pts',(1.01123236493507,1.,1.67648246776457));
#25563=CARTESIAN_POINT('Ctrl Pts',(1.01561026162786,1.,1.6804428989482));
#25564=CARTESIAN_POINT('Ctrl Pts',(1.02006795074222,1.,1.68440578021739));
#25565=CARTESIAN_POINT('Ctrl Pts',(1.02460180535272,1.,1.68836910178475));
#25566=CARTESIAN_POINT('Ctrl Pts',(1.02919977579155,1.,1.69231840863471));
#25567=CARTESIAN_POINT('Ctrl Pts',(1.03384646003587,1.,1.69623414782769));
#25568=CARTESIAN_POINT('Ctrl Pts',(1.03852922490782,1.,1.70010052930951));
#25569=CARTESIAN_POINT('Ctrl Pts',(1.04324363334546,1.,1.70391338707969));
#25570=CARTESIAN_POINT('Ctrl Pts',(1.0479908540499,1.,1.70767646263641));
#25571=CARTESIAN_POINT('Ctrl Pts',(1.05277517202853,1.,1.71139783543986));
#25572=CARTESIAN_POINT('Ctrl Pts',(1.05760163192481,1.,1.71508654427022));
#25573=CARTESIAN_POINT('Ctrl Pts',(1.06247324680649,1.,1.71874858456908));
#25574=CARTESIAN_POINT('Ctrl Pts',(1.06738966975463,1.,1.72238500928456));
#25575=CARTESIAN_POINT('Ctrl Pts',(1.07234866990252,1.,1.72599406198489));
#25576=CARTESIAN_POINT('Ctrl Pts',(1.0773470373727,1.,1.72957248977424));
#25577=CARTESIAN_POINT('Ctrl Pts',(1.08238162784749,1.,1.73311705663407));
#25578=CARTESIAN_POINT('Ctrl Pts',(1.08745056285429,1.,1.73662628326093));
#25579=CARTESIAN_POINT('Ctrl Pts',(1.09255329056496,1.,1.74010053962252));
#25580=CARTESIAN_POINT('Ctrl Pts',(1.09768999241229,1.,1.74354119236212));
#25581=CARTESIAN_POINT('Ctrl Pts',(1.10286118991144,1.,1.74695004214924));
#25582=CARTESIAN_POINT('Ctrl Pts',(1.10806728183003,1.,1.75032866075914));
#25583=CARTESIAN_POINT('Ctrl Pts',(1.11330807582542,1.,1.75367772094617));
#25584=CARTESIAN_POINT('Ctrl Pts',(1.11858293216752,1.,1.75699720772089));
#25585=CARTESIAN_POINT('Ctrl Pts',(1.12389096855078,1.,1.76028671825084));
#25586=CARTESIAN_POINT('Ctrl Pts',(1.12923123555076,1.,1.76354571966171));
#25587=CARTESIAN_POINT('Ctrl Pts',(1.13460291804634,1.,1.76677384551883));
#25588=CARTESIAN_POINT('Ctrl Pts',(1.14000548337,1.,1.76997111386806));
#25589=CARTESIAN_POINT('Ctrl Pts',(1.14543858226948,1.,1.77313777896234));
#25590=CARTESIAN_POINT('Ctrl Pts',(1.15090197841531,1.,1.77627422557034));
#25591=CARTESIAN_POINT('Ctrl Pts',(1.15639547194689,1.,1.77938085564261));
#25592=CARTESIAN_POINT('Ctrl Pts',(1.16191881298458,1.,1.78245795880949));
#25593=CARTESIAN_POINT('Ctrl Pts',(1.16747166312239,1.,1.78550566040349));
#25594=CARTESIAN_POINT('Ctrl Pts',(1.17305363177265,1.,1.78852398877523));
#25595=CARTESIAN_POINT('Ctrl Pts',(1.17866429440781,1.,1.79151291552646));
#25596=CARTESIAN_POINT('Ctrl Pts',(1.18430321697471,1.,1.79447240321572));
#25597=CARTESIAN_POINT('Ctrl Pts',(1.1899699793456,1.,1.79740245923649));
#25598=CARTESIAN_POINT('Ctrl Pts',(1.19566418930405,1.,1.80030314370121));
#25599=CARTESIAN_POINT('Ctrl Pts',(1.2013854893912,1.,1.8031745483882));
#25600=CARTESIAN_POINT('Ctrl Pts',(1.20713356605519,1.,1.80601678480772));
#25601=CARTESIAN_POINT('Ctrl Pts',(1.2129081570818,1.,1.80882996916931));
#25602=CARTESIAN_POINT('Ctrl Pts',(1.2187090610323,1.,1.81161420806172));
#25603=CARTESIAN_POINT('Ctrl Pts',(1.22453613304507,1.,1.81436959209778));
#25604=CARTESIAN_POINT('Ctrl Pts',(1.22921864890975,1.,1.81655087183054));
#25605=CARTESIAN_POINT('Ctrl Pts',(1.23274224526804,1.,1.81817389920914));
#25606=CARTESIAN_POINT('Ctrl Pts',(1.23509651170384,1.,1.81925017193531));
#25607=CARTESIAN_POINT('Ctrl Pts',(1.23627494547115,1.,1.81978687191668));
#25608=CARTESIAN_POINT('',(0.892032620296854,0.,1.5055822144029));
#25609=CARTESIAN_POINT('Origin',(0.,0.,0.));
#25610=CARTESIAN_POINT('',(0.693717979106305,1.,1.60662857109684));
#25611=CARTESIAN_POINT('Origin',(0.,1.,0.));
#25612=CARTESIAN_POINT('',(0.693717979106305,0.,1.60662857109684));
#25613=CARTESIAN_POINT('Ctrl Pts',(0.7455743247944,-1.,2.0698113262342));
#25614=CARTESIAN_POINT('Ctrl Pts',(0.7455743247944,1.,2.0698113262342));
#25615=CARTESIAN_POINT('Ctrl Pts',(0.745832791378367,-1.,2.06854248895728));
#25616=CARTESIAN_POINT('Ctrl Pts',(0.745832791378367,1.,2.06854248895728));
#25617=CARTESIAN_POINT('Ctrl Pts',(0.7463458715442,-1.,2.06600523016815));
#25618=CARTESIAN_POINT('Ctrl Pts',(0.7463458715442,1.,2.06600523016815));
#25619=CARTESIAN_POINT('Ctrl Pts',(0.747103932787919,-1.,2.06220058927826));
#25620=CARTESIAN_POINT('Ctrl Pts',(0.747103932787919,1.,2.06220058927826));
#25621=CARTESIAN_POINT('Ctrl Pts',(0.748091554183802,-1.,2.05713023031007));
#25622=CARTESIAN_POINT('Ctrl Pts',(0.748091554183802,1.,2.05713023031007));
#25623=CARTESIAN_POINT('Ctrl Pts',(0.749287468665046,-1.,2.05079645592154));
#25624=CARTESIAN_POINT('Ctrl Pts',(0.749287468665046,1.,2.05079645592154));
#25625=CARTESIAN_POINT('Ctrl Pts',(0.750444657875575,-1.,2.04446689147979));
#25626=CARTESIAN_POINT('Ctrl Pts',(0.750444657875575,1.,2.04446689147979));
#25627=CARTESIAN_POINT('Ctrl Pts',(0.751562963361115,-1.,2.03814160092099));
#25628=CARTESIAN_POINT('Ctrl Pts',(0.751562963361115,1.,2.03814160092099));
#25629=CARTESIAN_POINT('Ctrl Pts',(0.75264218048721,-1.,2.03182068456221));
#25630=CARTESIAN_POINT('Ctrl Pts',(0.75264218048721,1.,2.03182068456221));
#25631=CARTESIAN_POINT('Ctrl Pts',(0.753682061112768,-1.,2.02550428623313));
#25632=CARTESIAN_POINT('Ctrl Pts',(0.753682061112768,1.,2.02550428623313));
#25633=CARTESIAN_POINT('Ctrl Pts',(0.754682330722816,-1.,2.01919259405809));
#25634=CARTESIAN_POINT('Ctrl Pts',(0.754682330722816,1.,2.01919259405809));
#25635=CARTESIAN_POINT('Ctrl Pts',(0.755642704957865,-1.,2.01288584328084));
#25636=CARTESIAN_POINT('Ctrl Pts',(0.755642704957865,1.,2.01288584328084));
#25637=CARTESIAN_POINT('Ctrl Pts',(0.75656290464667,-1.,2.0065843158773));
#25638=CARTESIAN_POINT('Ctrl Pts',(0.75656290464667,1.,2.0065843158773));
#25639=CARTESIAN_POINT('Ctrl Pts',(0.757442676862724,-1.,2.00028834739178));
#25640=CARTESIAN_POINT('Ctrl Pts',(0.757442676862724,1.,2.00028834739178));
#25641=CARTESIAN_POINT('Ctrl Pts',(0.758281796766761,-1.,1.99399831098817));
#25642=CARTESIAN_POINT('Ctrl Pts',(0.758281796766761,1.,1.99399831098817));
#25643=CARTESIAN_POINT('Ctrl Pts',(0.759080037802488,-1.,1.98771456680874));
#25644=CARTESIAN_POINT('Ctrl Pts',(0.759080037802488,1.,1.98771456680874));
#25645=CARTESIAN_POINT('Ctrl Pts',(0.75983714745219,-1.,1.98143741418172));
#25646=CARTESIAN_POINT('Ctrl Pts',(0.75983714745219,1.,1.98143741418172));
#25647=CARTESIAN_POINT('Ctrl Pts',(0.760552825409757,-1.,1.97516705321494));
#25648=CARTESIAN_POINT('Ctrl Pts',(0.760552825409757,1.,1.97516705321494));
#25649=CARTESIAN_POINT('Ctrl Pts',(0.76122669048382,-1.,1.96890351582499));
#25650=CARTESIAN_POINT('Ctrl Pts',(0.76122669048382,1.,1.96890351582499));
#25651=CARTESIAN_POINT('Ctrl Pts',(0.761858300014423,-1.,1.96264672744186));
#25652=CARTESIAN_POINT('Ctrl Pts',(0.761858300014423,1.,1.96264672744186));
#25653=CARTESIAN_POINT('Ctrl Pts',(0.762447203806178,-1.,1.95639665309869));
#25654=CARTESIAN_POINT('Ctrl Pts',(0.762447203806178,1.,1.95639665309869));
#25655=CARTESIAN_POINT('Ctrl Pts',(0.762992990878769,-1.,1.95015342590024));
#25656=CARTESIAN_POINT('Ctrl Pts',(0.762992990878769,1.,1.95015342590024));
#25657=CARTESIAN_POINT('Ctrl Pts',(0.763495333538629,-1.,1.9439174661764));
#25658=CARTESIAN_POINT('Ctrl Pts',(0.763495333538629,1.,1.9439174661764));
#25659=CARTESIAN_POINT('Ctrl Pts',(0.763954049121458,-1.,1.93768964875886));
#25660=CARTESIAN_POINT('Ctrl Pts',(0.763954049121458,1.,1.93768964875886));
#25661=CARTESIAN_POINT('Ctrl Pts',(0.76436901067394,-1.,1.93147105496382));
#25662=CARTESIAN_POINT('Ctrl Pts',(0.76436901067394,1.,1.93147105496382));
#25663=CARTESIAN_POINT('Ctrl Pts',(0.764740025488211,-1.,1.92526263537048));
#25664=CARTESIAN_POINT('Ctrl Pts',(0.764740025488211,1.,1.92526263537048));
#25665=CARTESIAN_POINT('Ctrl Pts',(0.765066729667088,-1.,1.91906491634196));
#25666=CARTESIAN_POINT('Ctrl Pts',(0.765066729667088,1.,1.91906491634196));
#25667=CARTESIAN_POINT('Ctrl Pts',(0.765348465884722,-1.,1.91287765805169));
#25668=CARTESIAN_POINT('Ctrl Pts',(0.765348465884722,1.,1.91287765805169));
#25669=CARTESIAN_POINT('Ctrl Pts',(0.765584196937919,-1.,1.90669961402356));
#25670=CARTESIAN_POINT('Ctrl Pts',(0.765584196937919,1.,1.90669961402356));
#25671=CARTESIAN_POINT('Ctrl Pts',(0.765772772593386,-1.,1.90052930393596));
#25672=CARTESIAN_POINT('Ctrl Pts',(0.765772772593386,1.,1.90052930393596));
#25673=CARTESIAN_POINT('Ctrl Pts',(0.765913193856978,-1.,1.89436577771388));
#25674=CARTESIAN_POINT('Ctrl Pts',(0.765913193856978,1.,1.89436577771388));
#25675=CARTESIAN_POINT('Ctrl Pts',(0.766004837062091,-1.,1.88820926433409));
#25676=CARTESIAN_POINT('Ctrl Pts',(0.766004837062091,1.,1.88820926433409));
#25677=CARTESIAN_POINT('Ctrl Pts',(0.766047794851864,-1.,1.88206215302561));
#25678=CARTESIAN_POINT('Ctrl Pts',(0.766047794851864,1.,1.88206215302561));
#25679=CARTESIAN_POINT('Ctrl Pts',(0.766042837036744,-1.,1.87592888967883));
#25680=CARTESIAN_POINT('Ctrl Pts',(0.766042837036744,1.,1.87592888967883));
#25681=CARTESIAN_POINT('Ctrl Pts',(0.765990708546091,-1.,1.86981398314341));
#25682=CARTESIAN_POINT('Ctrl Pts',(0.765990708546091,1.,1.86981398314341));
#25683=CARTESIAN_POINT('Ctrl Pts',(0.765891519092547,-1.,1.86372027063312));
#25684=CARTESIAN_POINT('Ctrl Pts',(0.765891519092547,1.,1.86372027063312));
#25685=CARTESIAN_POINT('Ctrl Pts',(0.765744212909318,-1.,1.85764741390394));
#25686=CARTESIAN_POINT('Ctrl Pts',(0.765744212909318,1.,1.85764741390394));
#25687=CARTESIAN_POINT('Ctrl Pts',(0.765545710619062,-1.,1.85158945130063));
#25688=CARTESIAN_POINT('Ctrl Pts',(0.765545710619062,1.,1.85158945130063));
#25689=CARTESIAN_POINT('Ctrl Pts',(0.765291664862029,-1.,1.84553698875924));
#25690=CARTESIAN_POINT('Ctrl Pts',(0.765291664862029,1.,1.84553698875924));
#25691=CARTESIAN_POINT('Ctrl Pts',(0.764978057881737,-1.,1.83948181064835));
#25692=CARTESIAN_POINT('Ctrl Pts',(0.764978057881737,1.,1.83948181064835));
#25693=CARTESIAN_POINT('Ctrl Pts',(0.764602549687853,-1.,1.83342077227142));
#25694=CARTESIAN_POINT('Ctrl Pts',(0.764602549687853,1.,1.83342077227142));
#25695=CARTESIAN_POINT('Ctrl Pts',(0.764165902605995,-1.,1.82735991200065));
#25696=CARTESIAN_POINT('Ctrl Pts',(0.764165902605995,1.,1.82735991200065));
#25697=CARTESIAN_POINT('Ctrl Pts',(0.763673465462726,-1.,1.82131873145266));
#25698=CARTESIAN_POINT('Ctrl Pts',(0.763673465462726,1.,1.82131873145266));
#25699=CARTESIAN_POINT('Ctrl Pts',(0.763132003836634,-1.,1.8153211840553));
#25700=CARTESIAN_POINT('Ctrl Pts',(0.763132003836634,1.,1.8153211840553));
#25701=CARTESIAN_POINT('Ctrl Pts',(0.762546129463938,-1.,1.80938551463965));
#25702=CARTESIAN_POINT('Ctrl Pts',(0.762546129463938,1.,1.80938551463965));
#25703=CARTESIAN_POINT('Ctrl Pts',(0.761915336443547,-1.,1.80351583877342));
#25704=CARTESIAN_POINT('Ctrl Pts',(0.761915336443547,1.,1.80351583877342));
#25705=CARTESIAN_POINT('Ctrl Pts',(0.761229695230558,-1.,1.79768986997783));
#25706=CARTESIAN_POINT('Ctrl Pts',(0.761229695230558,1.,1.79768986997783));
#25707=CARTESIAN_POINT('Ctrl Pts',(0.760469555880749,-1.,1.7918581561088));
#25708=CARTESIAN_POINT('Ctrl Pts',(0.760469555880749,1.,1.7918581561088));
#25709=CARTESIAN_POINT('Ctrl Pts',(0.759614401110189,-1.,1.78596964884604));
#25710=CARTESIAN_POINT('Ctrl Pts',(0.759614401110189,1.,1.78596964884604));
#25711=CARTESIAN_POINT('Ctrl Pts',(0.758650626677518,-1.,1.77999411220945));
#25712=CARTESIAN_POINT('Ctrl Pts',(0.758650626677518,1.,1.77999411220945));
#25713=CARTESIAN_POINT('Ctrl Pts',(0.757578264077028,-1.,1.77394167108292));
#25714=CARTESIAN_POINT('Ctrl Pts',(0.757578264077028,1.,1.77394167108292));
#25715=CARTESIAN_POINT('Ctrl Pts',(0.75642189602781,-1.,1.76789396002998));
#25716=CARTESIAN_POINT('Ctrl Pts',(0.75642189602781,1.,1.76789396002998));
#25717=CARTESIAN_POINT('Ctrl Pts',(0.755220979974461,-1.,1.76197817240128));
#25718=CARTESIAN_POINT('Ctrl Pts',(0.755220979974461,1.,1.76197817240128));
#25719=CARTESIAN_POINT('Ctrl Pts',(0.754009254027828,-1.,1.75631083600019));
#25720=CARTESIAN_POINT('Ctrl Pts',(0.754009254027828,1.,1.75631083600019));
#25721=CARTESIAN_POINT('Ctrl Pts',(0.752797683531314,-1.,1.75095139468794));
#25722=CARTESIAN_POINT('Ctrl Pts',(0.752797683531314,1.,1.75095139468794));
#25723=CARTESIAN_POINT('Ctrl Pts',(0.751555614164482,-1.,1.74585086852502));
#25724=CARTESIAN_POINT('Ctrl Pts',(0.751555614164482,1.,1.74585086852502));
#25725=CARTESIAN_POINT('Ctrl Pts',(0.750193435981249,-1.,1.74080458267114));
#25726=CARTESIAN_POINT('Ctrl Pts',(0.750193435981249,1.,1.74080458267114));
#25727=CARTESIAN_POINT('Ctrl Pts',(0.74858246295687,-1.,1.7355035168033));
#25728=CARTESIAN_POINT('Ctrl Pts',(0.74858246295687,1.,1.7355035168033));
#25729=CARTESIAN_POINT('Ctrl Pts',(0.746574710097752,-1.,1.72958533647714));
#25730=CARTESIAN_POINT('Ctrl Pts',(0.746574710097752,1.,1.72958533647714));
#25731=CARTESIAN_POINT('Ctrl Pts',(0.744021445433093,-1.,1.72268229916769));
#25732=CARTESIAN_POINT('Ctrl Pts',(0.744021445433093,1.,1.72268229916769));
#25733=CARTESIAN_POINT('Ctrl Pts',(0.74079516202821,-1.,1.71447789751001));
#25734=CARTESIAN_POINT('Ctrl Pts',(0.74079516202821,1.,1.71447789751001));
#25735=CARTESIAN_POINT('Ctrl Pts',(0.736799665716932,-1.,1.70473309004249));
#25736=CARTESIAN_POINT('Ctrl Pts',(0.736799665716932,1.,1.70473309004249));
#25737=CARTESIAN_POINT('Ctrl Pts',(0.731963238685357,-1.,1.69326921972915));
#25738=CARTESIAN_POINT('Ctrl Pts',(0.731963238685357,1.,1.69326921972915));
#25739=CARTESIAN_POINT('Ctrl Pts',(0.726235967982445,-1.,1.67996158451922));
#25740=CARTESIAN_POINT('Ctrl Pts',(0.726235967982445,1.,1.67996158451922));
#25741=CARTESIAN_POINT('Ctrl Pts',(0.719585433787949,-1.,1.66472880551777));
#25742=CARTESIAN_POINT('Ctrl Pts',(0.719585433787949,1.,1.66472880551777));
#25743=CARTESIAN_POINT('Ctrl Pts',(0.711993139340447,-1.,1.64752408828442));
#25744=CARTESIAN_POINT('Ctrl Pts',(0.711993139340447,1.,1.64752408828442));
#25745=CARTESIAN_POINT('Ctrl Pts',(0.705159151977294,-1.,1.6321654166204));
#25746=CARTESIAN_POINT('Ctrl Pts',(0.705159151977294,1.,1.6321654166204));
#25747=CARTESIAN_POINT('Ctrl Pts',(0.699605146398836,-1.,1.61974673471117));
#25748=CARTESIAN_POINT('Ctrl Pts',(0.699605146398836,1.,1.61974673471117));
#25749=CARTESIAN_POINT('Ctrl Pts',(0.69571209787897,-1.,1.61106790957619));
#25750=CARTESIAN_POINT('Ctrl Pts',(0.69571209787897,1.,1.61106790957619));
#25751=CARTESIAN_POINT('Ctrl Pts',(0.693717979106305,-1.,1.60662857109684));
#25752=CARTESIAN_POINT('Ctrl Pts',(0.693717979106305,1.,1.60662857109684));
#25753=CARTESIAN_POINT('',(0.7455743247944,1.,2.0698113262342));
#25754=CARTESIAN_POINT('Ctrl Pts',(0.7455743247944,1.,2.0698113262342));
#25755=CARTESIAN_POINT('Ctrl Pts',(0.745832791378367,1.,2.06854248895728));
#25756=CARTESIAN_POINT('Ctrl Pts',(0.7463458715442,1.,2.06600523016815));
#25757=CARTESIAN_POINT('Ctrl Pts',(0.747103932787919,1.,2.06220058927826));
#25758=CARTESIAN_POINT('Ctrl Pts',(0.748091554183802,1.,2.05713023031007));
#25759=CARTESIAN_POINT('Ctrl Pts',(0.749287468665046,1.,2.05079645592154));
#25760=CARTESIAN_POINT('Ctrl Pts',(0.750444657875575,1.,2.04446689147979));
#25761=CARTESIAN_POINT('Ctrl Pts',(0.751562963361115,1.,2.03814160092099));
#25762=CARTESIAN_POINT('Ctrl Pts',(0.75264218048721,1.,2.03182068456221));
#25763=CARTESIAN_POINT('Ctrl Pts',(0.753682061112768,1.,2.02550428623313));
#25764=CARTESIAN_POINT('Ctrl Pts',(0.754682330722816,1.,2.01919259405809));
#25765=CARTESIAN_POINT('Ctrl Pts',(0.755642704957865,1.,2.01288584328084));
#25766=CARTESIAN_POINT('Ctrl Pts',(0.75656290464667,1.,2.0065843158773));
#25767=CARTESIAN_POINT('Ctrl Pts',(0.757442676862724,1.,2.00028834739178));
#25768=CARTESIAN_POINT('Ctrl Pts',(0.758281796766761,1.,1.99399831098817));
#25769=CARTESIAN_POINT('Ctrl Pts',(0.759080037802488,1.,1.98771456680874));
#25770=CARTESIAN_POINT('Ctrl Pts',(0.75983714745219,1.,1.98143741418172));
#25771=CARTESIAN_POINT('Ctrl Pts',(0.760552825409757,1.,1.97516705321494));
#25772=CARTESIAN_POINT('Ctrl Pts',(0.76122669048382,1.,1.96890351582499));
#25773=CARTESIAN_POINT('Ctrl Pts',(0.761858300014423,1.,1.96264672744186));
#25774=CARTESIAN_POINT('Ctrl Pts',(0.762447203806178,1.,1.95639665309869));
#25775=CARTESIAN_POINT('Ctrl Pts',(0.762992990878769,1.,1.95015342590024));
#25776=CARTESIAN_POINT('Ctrl Pts',(0.763495333538629,1.,1.9439174661764));
#25777=CARTESIAN_POINT('Ctrl Pts',(0.763954049121458,1.,1.93768964875886));
#25778=CARTESIAN_POINT('Ctrl Pts',(0.76436901067394,1.,1.93147105496382));
#25779=CARTESIAN_POINT('Ctrl Pts',(0.764740025488211,1.,1.92526263537048));
#25780=CARTESIAN_POINT('Ctrl Pts',(0.765066729667088,1.,1.91906491634196));
#25781=CARTESIAN_POINT('Ctrl Pts',(0.765348465884722,1.,1.91287765805169));
#25782=CARTESIAN_POINT('Ctrl Pts',(0.765584196937919,1.,1.90669961402356));
#25783=CARTESIAN_POINT('Ctrl Pts',(0.765772772593386,1.,1.90052930393596));
#25784=CARTESIAN_POINT('Ctrl Pts',(0.765913193856978,1.,1.89436577771388));
#25785=CARTESIAN_POINT('Ctrl Pts',(0.766004837062091,1.,1.88820926433409));
#25786=CARTESIAN_POINT('Ctrl Pts',(0.766047794851864,1.,1.88206215302561));
#25787=CARTESIAN_POINT('Ctrl Pts',(0.766042837036744,1.,1.87592888967883));
#25788=CARTESIAN_POINT('Ctrl Pts',(0.765990708546091,1.,1.86981398314341));
#25789=CARTESIAN_POINT('Ctrl Pts',(0.765891519092547,1.,1.86372027063312));
#25790=CARTESIAN_POINT('Ctrl Pts',(0.765744212909318,1.,1.85764741390394));
#25791=CARTESIAN_POINT('Ctrl Pts',(0.765545710619062,1.,1.85158945130063));
#25792=CARTESIAN_POINT('Ctrl Pts',(0.765291664862029,1.,1.84553698875924));
#25793=CARTESIAN_POINT('Ctrl Pts',(0.764978057881737,1.,1.83948181064835));
#25794=CARTESIAN_POINT('Ctrl Pts',(0.764602549687853,1.,1.83342077227142));
#25795=CARTESIAN_POINT('Ctrl Pts',(0.764165902605995,1.,1.82735991200065));
#25796=CARTESIAN_POINT('Ctrl Pts',(0.763673465462726,1.,1.82131873145266));
#25797=CARTESIAN_POINT('Ctrl Pts',(0.763132003836634,1.,1.8153211840553));
#25798=CARTESIAN_POINT('Ctrl Pts',(0.762546129463938,1.,1.80938551463965));
#25799=CARTESIAN_POINT('Ctrl Pts',(0.761915336443547,1.,1.80351583877342));
#25800=CARTESIAN_POINT('Ctrl Pts',(0.761229695230558,1.,1.79768986997783));
#25801=CARTESIAN_POINT('Ctrl Pts',(0.760469555880749,1.,1.7918581561088));
#25802=CARTESIAN_POINT('Ctrl Pts',(0.759614401110189,1.,1.78596964884604));
#25803=CARTESIAN_POINT('Ctrl Pts',(0.758650626677518,1.,1.77999411220945));
#25804=CARTESIAN_POINT('Ctrl Pts',(0.757578264077028,1.,1.77394167108292));
#25805=CARTESIAN_POINT('Ctrl Pts',(0.75642189602781,1.,1.76789396002998));
#25806=CARTESIAN_POINT('Ctrl Pts',(0.755220979974461,1.,1.76197817240128));
#25807=CARTESIAN_POINT('Ctrl Pts',(0.754009254027828,1.,1.75631083600019));
#25808=CARTESIAN_POINT('Ctrl Pts',(0.752797683531314,1.,1.75095139468794));
#25809=CARTESIAN_POINT('Ctrl Pts',(0.751555614164482,1.,1.74585086852502));
#25810=CARTESIAN_POINT('Ctrl Pts',(0.750193435981249,1.,1.74080458267114));
#25811=CARTESIAN_POINT('Ctrl Pts',(0.74858246295687,1.,1.7355035168033));
#25812=CARTESIAN_POINT('Ctrl Pts',(0.746574710097752,1.,1.72958533647714));
#25813=CARTESIAN_POINT('Ctrl Pts',(0.744021445433093,1.,1.72268229916769));
#25814=CARTESIAN_POINT('Ctrl Pts',(0.74079516202821,1.,1.71447789751001));
#25815=CARTESIAN_POINT('Ctrl Pts',(0.736799665716932,1.,1.70473309004249));
#25816=CARTESIAN_POINT('Ctrl Pts',(0.731963238685357,1.,1.69326921972915));
#25817=CARTESIAN_POINT('Ctrl Pts',(0.726235967982445,1.,1.67996158451922));
#25818=CARTESIAN_POINT('Ctrl Pts',(0.719585433787949,1.,1.66472880551777));
#25819=CARTESIAN_POINT('Ctrl Pts',(0.711993139340447,1.,1.64752408828442));
#25820=CARTESIAN_POINT('Ctrl Pts',(0.705159151977294,1.,1.6321654166204));
#25821=CARTESIAN_POINT('Ctrl Pts',(0.699605146398836,1.,1.61974673471117));
#25822=CARTESIAN_POINT('Ctrl Pts',(0.69571209787897,1.,1.61106790957619));
#25823=CARTESIAN_POINT('Ctrl Pts',(0.693717979106305,1.,1.60662857109684));
#25824=CARTESIAN_POINT('',(0.7455743247944,0.,2.0698113262342));
#25825=CARTESIAN_POINT('Origin',(0.61342227326009,0.,2.11275013067528));
#25826=CARTESIAN_POINT('',(0.61342227326009,1.,2.11275013067528));
#25827=CARTESIAN_POINT('',(0.7455743247944,1.,2.0698113262342));
#25828=CARTESIAN_POINT('',(0.61342227326009,0.,2.11275013067528));
#25829=CARTESIAN_POINT('Ctrl Pts',(0.383122945602004,-1.,1.7075470150345));
#25830=CARTESIAN_POINT('Ctrl Pts',(0.383122945602004,1.,1.7075470150345));
#25831=CARTESIAN_POINT('Ctrl Pts',(0.384119047315541,-1.,1.71231062891958));
#25832=CARTESIAN_POINT('Ctrl Pts',(0.384119047315541,1.,1.71231062891958));
#25833=CARTESIAN_POINT('Ctrl Pts',(0.38607079032701,-1.,1.72162022246158));
#25834=CARTESIAN_POINT('Ctrl Pts',(0.38607079032701,1.,1.72162022246158));
#25835=CARTESIAN_POINT('Ctrl Pts',(0.388877023509191,-1.,1.7349317097561));
#25836=CARTESIAN_POINT('Ctrl Pts',(0.388877023509191,1.,1.7349317097561));
#25837=CARTESIAN_POINT('Ctrl Pts',(0.392375812294307,-1.,1.75137405313962));
#25838=CARTESIAN_POINT('Ctrl Pts',(0.392375812294307,1.,1.75137405313962));
#25839=CARTESIAN_POINT('Ctrl Pts',(0.39634619612042,-1.,1.7697556004756));
#25840=CARTESIAN_POINT('Ctrl Pts',(0.39634619612042,1.,1.7697556004756));
#25841=CARTESIAN_POINT('Ctrl Pts',(0.39991940378308,-1.,1.78598826347533));
#25842=CARTESIAN_POINT('Ctrl Pts',(0.39991940378308,1.,1.78598826347533));
#25843=CARTESIAN_POINT('Ctrl Pts',(0.403107976170441,-1.,1.80012077176221));
#25844=CARTESIAN_POINT('Ctrl Pts',(0.403107976170441,1.,1.80012077176221));
#25845=CARTESIAN_POINT('Ctrl Pts',(0.405933518411838,-1.,1.81223801813988));
#25846=CARTESIAN_POINT('Ctrl Pts',(0.405933518411838,1.,1.81223801813988));
#25847=CARTESIAN_POINT('Ctrl Pts',(0.408428948108533,-1.,1.8224702267854));
#25848=CARTESIAN_POINT('Ctrl Pts',(0.408428948108533,1.,1.8224702267854));
#25849=CARTESIAN_POINT('Ctrl Pts',(0.410641256301674,-1.,1.83100408895216));
#25850=CARTESIAN_POINT('Ctrl Pts',(0.410641256301674,1.,1.83100408895216));
#25851=CARTESIAN_POINT('Ctrl Pts',(0.412633125322161,-1.,1.83808953475839));
#25852=CARTESIAN_POINT('Ctrl Pts',(0.412633125322161,1.,1.83808953475839));
#25853=CARTESIAN_POINT('Ctrl Pts',(0.41448743825434,-1.,1.8440575707371));
#25854=CARTESIAN_POINT('Ctrl Pts',(0.41448743825434,1.,1.8440575707371));
#25855=CARTESIAN_POINT('Ctrl Pts',(0.416300022038864,-1.,1.84929312929882));
#25856=CARTESIAN_POINT('Ctrl Pts',(0.416300022038864,1.,1.84929312929882));
#25857=CARTESIAN_POINT('Ctrl Pts',(0.418164129143534,-1.,1.85417632856234));
#25858=CARTESIAN_POINT('Ctrl Pts',(0.418164129143534,1.,1.85417632856234));
#25859=CARTESIAN_POINT('Ctrl Pts',(0.420157287975619,-1.,1.85903281096686));
#25860=CARTESIAN_POINT('Ctrl Pts',(0.420157287975619,1.,1.85903281096686));
#25861=CARTESIAN_POINT('Ctrl Pts',(0.422327307418275,-1.,1.86408083334028));
#25862=CARTESIAN_POINT('Ctrl Pts',(0.422327307418275,1.,1.86408083334028));
#25863=CARTESIAN_POINT('Ctrl Pts',(0.424678177291358,-1.,1.86937803944323));
#25864=CARTESIAN_POINT('Ctrl Pts',(0.424678177291358,1.,1.86937803944323));
#25865=CARTESIAN_POINT('Ctrl Pts',(0.427183828519102,-1.,1.87486989291484));
#25866=CARTESIAN_POINT('Ctrl Pts',(0.427183828519102,1.,1.87486989291484));
#25867=CARTESIAN_POINT('Ctrl Pts',(0.429803062482344,-1.,1.88044229001832));
#25868=CARTESIAN_POINT('Ctrl Pts',(0.429803062482344,1.,1.88044229001832));
#25869=CARTESIAN_POINT('Ctrl Pts',(0.432493038548748,-1.,1.88596913666793));
#25870=CARTESIAN_POINT('Ctrl Pts',(0.432493038548748,1.,1.88596913666793));
#25871=CARTESIAN_POINT('Ctrl Pts',(0.435225660963383,-1.,1.89136993975504));
#25872=CARTESIAN_POINT('Ctrl Pts',(0.435225660963383,1.,1.89136993975504));
#25873=CARTESIAN_POINT('Ctrl Pts',(0.437995003948244,-1.,1.89663648956466));
#25874=CARTESIAN_POINT('Ctrl Pts',(0.437995003948244,1.,1.89663648956466));
#25875=CARTESIAN_POINT('Ctrl Pts',(0.440807833704038,-1.,1.90180124389086));
#25876=CARTESIAN_POINT('Ctrl Pts',(0.440807833704038,1.,1.90180124389086));
#25877=CARTESIAN_POINT('Ctrl Pts',(0.44367755684915,-1.,1.90691756144898));
#25878=CARTESIAN_POINT('Ctrl Pts',(0.44367755684915,1.,1.90691756144898));
#25879=CARTESIAN_POINT('Ctrl Pts',(0.446617343485711,-1.,1.9120369998112));
#25880=CARTESIAN_POINT('Ctrl Pts',(0.446617343485711,1.,1.9120369998112));
#25881=CARTESIAN_POINT('Ctrl Pts',(0.449632260106662,-1.,1.91718342555755));
#25882=CARTESIAN_POINT('Ctrl Pts',(0.449632260106662,1.,1.91718342555755));
#25883=CARTESIAN_POINT('Ctrl Pts',(0.452719478359432,-1.,1.92235380648502));
#25884=CARTESIAN_POINT('Ctrl Pts',(0.452719478359432,1.,1.92235380648502));
#25885=CARTESIAN_POINT('Ctrl Pts',(0.45587200517437,-1.,1.92753067150476));
#25886=CARTESIAN_POINT('Ctrl Pts',(0.45587200517437,1.,1.92753067150476));
#25887=CARTESIAN_POINT('Ctrl Pts',(0.459081234547926,-1.,1.93269066517934));
#25888=CARTESIAN_POINT('Ctrl Pts',(0.459081234547926,1.,1.93269066517934));
#25889=CARTESIAN_POINT('Ctrl Pts',(0.462340031009056,-1.,1.93781486640821));
#25890=CARTESIAN_POINT('Ctrl Pts',(0.462340031009056,1.,1.93781486640821));
#25891=CARTESIAN_POINT('Ctrl Pts',(0.46564546202603,-1.,1.9428979419619));
#25892=CARTESIAN_POINT('Ctrl Pts',(0.46564546202603,1.,1.9428979419619));
#25893=CARTESIAN_POINT('Ctrl Pts',(0.468997482913135,-1.,1.94794381136514));
#25894=CARTESIAN_POINT('Ctrl Pts',(0.468997482913135,1.,1.94794381136514));
#25895=CARTESIAN_POINT('Ctrl Pts',(0.472397672264072,-1.,1.95296148278133));
#25896=CARTESIAN_POINT('Ctrl Pts',(0.472397672264072,1.,1.95296148278133));
#25897=CARTESIAN_POINT('Ctrl Pts',(0.475848034683176,-1.,1.95796111148177));
#25898=CARTESIAN_POINT('Ctrl Pts',(0.475848034683176,1.,1.95796111148177));
#25899=CARTESIAN_POINT('Ctrl Pts',(0.479349583074855,-1.,1.96294933055943));
#25900=CARTESIAN_POINT('Ctrl Pts',(0.479349583074855,1.,1.96294933055943));
#25901=CARTESIAN_POINT('Ctrl Pts',(0.48290166212069,-1.,1.96792703422362));
#25902=CARTESIAN_POINT('Ctrl Pts',(0.48290166212069,1.,1.96792703422362));
#25903=CARTESIAN_POINT('Ctrl Pts',(0.486502692907658,-1.,1.97289186263272));
#25904=CARTESIAN_POINT('Ctrl Pts',(0.486502692907658,1.,1.97289186263272));
#25905=CARTESIAN_POINT('Ctrl Pts',(0.490150627860952,-1.,1.97783973019229));
#25906=CARTESIAN_POINT('Ctrl Pts',(0.490150627860952,1.,1.97783973019229));
#25907=CARTESIAN_POINT('Ctrl Pts',(0.493843476541494,-1.,1.98276658761821));
#25908=CARTESIAN_POINT('Ctrl Pts',(0.493843476541494,1.,1.98276658761821));
#25909=CARTESIAN_POINT('Ctrl Pts',(0.497579909545574,-1.,1.98767044752932));
#25910=CARTESIAN_POINT('Ctrl Pts',(0.497579909545574,1.,1.98767044752932));
#25911=CARTESIAN_POINT('Ctrl Pts',(0.501359287727146,-1.,1.99255149126155));
#25912=CARTESIAN_POINT('Ctrl Pts',(0.501359287727146,1.,1.99255149126155));
#25913=CARTESIAN_POINT('Ctrl Pts',(0.505181361323026,-1.,1.99741107463572));
#25914=CARTESIAN_POINT('Ctrl Pts',(0.505181361323026,1.,1.99741107463572));
#25915=CARTESIAN_POINT('Ctrl Pts',(0.509046069886157,-1.,2.00225107134734));
#25916=CARTESIAN_POINT('Ctrl Pts',(0.509046069886157,1.,2.00225107134734));
#25917=CARTESIAN_POINT('Ctrl Pts',(0.512953306961792,-1.,2.00707309946949));
#25918=CARTESIAN_POINT('Ctrl Pts',(0.512953306961792,1.,2.00707309946949));
#25919=CARTESIAN_POINT('Ctrl Pts',(0.516902681728687,-1.,2.01187773939242));
#25920=CARTESIAN_POINT('Ctrl Pts',(0.516902681728687,1.,2.01187773939242));
#25921=CARTESIAN_POINT('Ctrl Pts',(0.52089359039937,-1.,2.01666477917286));
#25922=CARTESIAN_POINT('Ctrl Pts',(0.52089359039937,1.,2.01666477917286));
#25923=CARTESIAN_POINT('Ctrl Pts',(0.524925318333476,-1.,2.02143356304698));
#25924=CARTESIAN_POINT('Ctrl Pts',(0.524925318333476,1.,2.02143356304698));
#25925=CARTESIAN_POINT('Ctrl Pts',(0.528997127241914,-1.,2.0261832908329));
#25926=CARTESIAN_POINT('Ctrl Pts',(0.528997127241914,1.,2.0261832908329));
#25927=CARTESIAN_POINT('Ctrl Pts',(0.533108355132976,-1.,2.03091336214426));
#25928=CARTESIAN_POINT('Ctrl Pts',(0.533108355132976,1.,2.03091336214426));
#25929=CARTESIAN_POINT('Ctrl Pts',(0.537258489833262,-1.,2.03562362954037));
#25930=CARTESIAN_POINT('Ctrl Pts',(0.537258489833262,1.,2.03562362954037));
#25931=CARTESIAN_POINT('Ctrl Pts',(0.541447120615659,-1.,2.04031422690527));
#25932=CARTESIAN_POINT('Ctrl Pts',(0.541447120615659,1.,2.04031422690527));
#25933=CARTESIAN_POINT('Ctrl Pts',(0.54567390381743,-1.,2.04498544714588));
#25934=CARTESIAN_POINT('Ctrl Pts',(0.54567390381743,1.,2.04498544714588));
#25935=CARTESIAN_POINT('Ctrl Pts',(0.549938525150295,-1.,2.04963761077958));
#25936=CARTESIAN_POINT('Ctrl Pts',(0.549938525150295,1.,2.04963761077958));
#25937=CARTESIAN_POINT('Ctrl Pts',(0.554240657463906,-1.,2.05427091604413));
#25938=CARTESIAN_POINT('Ctrl Pts',(0.554240657463906,1.,2.05427091604413));
#25939=CARTESIAN_POINT('Ctrl Pts',(0.558579940185151,-1.,2.05888537756462));
#25940=CARTESIAN_POINT('Ctrl Pts',(0.558579940185151,1.,2.05888537756462));
#25941=CARTESIAN_POINT('Ctrl Pts',(0.562955993082261,-1.,2.06348090160589));
#25942=CARTESIAN_POINT('Ctrl Pts',(0.562955993082261,1.,2.06348090160589));
#25943=CARTESIAN_POINT('Ctrl Pts',(0.567368421181087,-1.,2.06805732997334));
#25944=CARTESIAN_POINT('Ctrl Pts',(0.567368421181087,1.,2.06805732997334));
#25945=CARTESIAN_POINT('Ctrl Pts',(0.571816823242602,-1.,2.07261449292824));
#25946=CARTESIAN_POINT('Ctrl Pts',(0.571816823242602,1.,2.07261449292824));
#25947=CARTESIAN_POINT('Ctrl Pts',(0.576300797416844,-1.,2.07715226767559));
#25948=CARTESIAN_POINT('Ctrl Pts',(0.576300797416844,1.,2.07715226767559));
#25949=CARTESIAN_POINT('Ctrl Pts',(0.580819952108063,-1.,2.08167059018418));
#25950=CARTESIAN_POINT('Ctrl Pts',(0.580819952108063,1.,2.08167059018418));
#25951=CARTESIAN_POINT('Ctrl Pts',(0.585373918991617,-1.,2.08616943727951));
#25952=CARTESIAN_POINT('Ctrl Pts',(0.585373918991617,1.,2.08616943727951));
#25953=CARTESIAN_POINT('Ctrl Pts',(0.589962365403406,-1.,2.09064881812129));
#25954=CARTESIAN_POINT('Ctrl Pts',(0.589962365403406,1.,2.09064881812129));
#25955=CARTESIAN_POINT('Ctrl Pts',(0.594585006052162,-1.,2.0951087622027));
#25956=CARTESIAN_POINT('Ctrl Pts',(0.594585006052162,1.,2.0951087622027));
#25957=CARTESIAN_POINT('Ctrl Pts',(0.599241616420533,-1.,2.0995493086477));
#25958=CARTESIAN_POINT('Ctrl Pts',(0.599241616420533,1.,2.0995493086477));
#25959=CARTESIAN_POINT('Ctrl Pts',(0.60393203073603,-1.,2.10397049886949));
#25960=CARTESIAN_POINT('Ctrl Pts',(0.60393203073603,1.,2.10397049886949));
#25961=CARTESIAN_POINT('Ctrl Pts',(0.607711315454876,-1.,2.1074919961518));
#25962=CARTESIAN_POINT('Ctrl Pts',(0.607711315454876,1.,2.1074919961518));
#25963=CARTESIAN_POINT('Ctrl Pts',(0.610560911689898,-1.,2.11012443807238));
#25964=CARTESIAN_POINT('Ctrl Pts',(0.610560911689898,1.,2.11012443807238));
#25965=CARTESIAN_POINT('Ctrl Pts',(0.6124673655618,-1.,2.11187554259986));
#25966=CARTESIAN_POINT('Ctrl Pts',(0.6124673655618,1.,2.11187554259986));
#25967=CARTESIAN_POINT('Ctrl Pts',(0.61342227326009,-1.,2.11275013067528));
#25968=CARTESIAN_POINT('Ctrl Pts',(0.61342227326009,1.,2.11275013067528));
#25969=CARTESIAN_POINT('',(0.383122945602004,1.,1.7075470150345));
#25970=CARTESIAN_POINT('Ctrl Pts',(0.383122945602004,1.,1.7075470150345));
#25971=CARTESIAN_POINT('Ctrl Pts',(0.384119047315541,1.,1.71231062891958));
#25972=CARTESIAN_POINT('Ctrl Pts',(0.38607079032701,1.,1.72162022246158));
#25973=CARTESIAN_POINT('Ctrl Pts',(0.388877023509191,1.,1.7349317097561));
#25974=CARTESIAN_POINT('Ctrl Pts',(0.392375812294307,1.,1.75137405313962));
#25975=CARTESIAN_POINT('Ctrl Pts',(0.39634619612042,1.,1.7697556004756));
#25976=CARTESIAN_POINT('Ctrl Pts',(0.39991940378308,1.,1.78598826347533));
#25977=CARTESIAN_POINT('Ctrl Pts',(0.403107976170441,1.,1.80012077176221));
#25978=CARTESIAN_POINT('Ctrl Pts',(0.405933518411838,1.,1.81223801813988));
#25979=CARTESIAN_POINT('Ctrl Pts',(0.408428948108533,1.,1.8224702267854));
#25980=CARTESIAN_POINT('Ctrl Pts',(0.410641256301674,1.,1.83100408895216));
#25981=CARTESIAN_POINT('Ctrl Pts',(0.412633125322161,1.,1.83808953475839));
#25982=CARTESIAN_POINT('Ctrl Pts',(0.41448743825434,1.,1.8440575707371));
#25983=CARTESIAN_POINT('Ctrl Pts',(0.416300022038864,1.,1.84929312929882));
#25984=CARTESIAN_POINT('Ctrl Pts',(0.418164129143534,1.,1.85417632856234));
#25985=CARTESIAN_POINT('Ctrl Pts',(0.420157287975619,1.,1.85903281096686));
#25986=CARTESIAN_POINT('Ctrl Pts',(0.422327307418275,1.,1.86408083334028));
#25987=CARTESIAN_POINT('Ctrl Pts',(0.424678177291358,1.,1.86937803944323));
#25988=CARTESIAN_POINT('Ctrl Pts',(0.427183828519102,1.,1.87486989291484));
#25989=CARTESIAN_POINT('Ctrl Pts',(0.429803062482344,1.,1.88044229001832));
#25990=CARTESIAN_POINT('Ctrl Pts',(0.432493038548748,1.,1.88596913666793));
#25991=CARTESIAN_POINT('Ctrl Pts',(0.435225660963383,1.,1.89136993975504));
#25992=CARTESIAN_POINT('Ctrl Pts',(0.437995003948244,1.,1.89663648956466));
#25993=CARTESIAN_POINT('Ctrl Pts',(0.440807833704038,1.,1.90180124389086));
#25994=CARTESIAN_POINT('Ctrl Pts',(0.44367755684915,1.,1.90691756144898));
#25995=CARTESIAN_POINT('Ctrl Pts',(0.446617343485711,1.,1.9120369998112));
#25996=CARTESIAN_POINT('Ctrl Pts',(0.449632260106662,1.,1.91718342555755));
#25997=CARTESIAN_POINT('Ctrl Pts',(0.452719478359432,1.,1.92235380648502));
#25998=CARTESIAN_POINT('Ctrl Pts',(0.45587200517437,1.,1.92753067150476));
#25999=CARTESIAN_POINT('Ctrl Pts',(0.459081234547926,1.,1.93269066517934));
#26000=CARTESIAN_POINT('Ctrl Pts',(0.462340031009056,1.,1.93781486640821));
#26001=CARTESIAN_POINT('Ctrl Pts',(0.46564546202603,1.,1.9428979419619));
#26002=CARTESIAN_POINT('Ctrl Pts',(0.468997482913135,1.,1.94794381136514));
#26003=CARTESIAN_POINT('Ctrl Pts',(0.472397672264072,1.,1.95296148278133));
#26004=CARTESIAN_POINT('Ctrl Pts',(0.475848034683176,1.,1.95796111148177));
#26005=CARTESIAN_POINT('Ctrl Pts',(0.479349583074855,1.,1.96294933055943));
#26006=CARTESIAN_POINT('Ctrl Pts',(0.48290166212069,1.,1.96792703422362));
#26007=CARTESIAN_POINT('Ctrl Pts',(0.486502692907658,1.,1.97289186263272));
#26008=CARTESIAN_POINT('Ctrl Pts',(0.490150627860952,1.,1.97783973019229));
#26009=CARTESIAN_POINT('Ctrl Pts',(0.493843476541494,1.,1.98276658761821));
#26010=CARTESIAN_POINT('Ctrl Pts',(0.497579909545574,1.,1.98767044752932));
#26011=CARTESIAN_POINT('Ctrl Pts',(0.501359287727146,1.,1.99255149126155));
#26012=CARTESIAN_POINT('Ctrl Pts',(0.505181361323026,1.,1.99741107463572));
#26013=CARTESIAN_POINT('Ctrl Pts',(0.509046069886157,1.,2.00225107134734));
#26014=CARTESIAN_POINT('Ctrl Pts',(0.512953306961792,1.,2.00707309946949));
#26015=CARTESIAN_POINT('Ctrl Pts',(0.516902681728687,1.,2.01187773939242));
#26016=CARTESIAN_POINT('Ctrl Pts',(0.52089359039937,1.,2.01666477917286));
#26017=CARTESIAN_POINT('Ctrl Pts',(0.524925318333476,1.,2.02143356304698));
#26018=CARTESIAN_POINT('Ctrl Pts',(0.528997127241914,1.,2.0261832908329));
#26019=CARTESIAN_POINT('Ctrl Pts',(0.533108355132976,1.,2.03091336214426));
#26020=CARTESIAN_POINT('Ctrl Pts',(0.537258489833262,1.,2.03562362954037));
#26021=CARTESIAN_POINT('Ctrl Pts',(0.541447120615659,1.,2.04031422690527));
#26022=CARTESIAN_POINT('Ctrl Pts',(0.54567390381743,1.,2.04498544714588));
#26023=CARTESIAN_POINT('Ctrl Pts',(0.549938525150295,1.,2.04963761077958));
#26024=CARTESIAN_POINT('Ctrl Pts',(0.554240657463906,1.,2.05427091604413));
#26025=CARTESIAN_POINT('Ctrl Pts',(0.558579940185151,1.,2.05888537756462));
#26026=CARTESIAN_POINT('Ctrl Pts',(0.562955993082261,1.,2.06348090160589));
#26027=CARTESIAN_POINT('Ctrl Pts',(0.567368421181087,1.,2.06805732997334));
#26028=CARTESIAN_POINT('Ctrl Pts',(0.571816823242602,1.,2.07261449292824));
#26029=CARTESIAN_POINT('Ctrl Pts',(0.576300797416844,1.,2.07715226767559));
#26030=CARTESIAN_POINT('Ctrl Pts',(0.580819952108063,1.,2.08167059018418));
#26031=CARTESIAN_POINT('Ctrl Pts',(0.585373918991617,1.,2.08616943727951));
#26032=CARTESIAN_POINT('Ctrl Pts',(0.589962365403406,1.,2.09064881812129));
#26033=CARTESIAN_POINT('Ctrl Pts',(0.594585006052162,1.,2.0951087622027));
#26034=CARTESIAN_POINT('Ctrl Pts',(0.599241616420533,1.,2.0995493086477));
#26035=CARTESIAN_POINT('Ctrl Pts',(0.60393203073603,1.,2.10397049886949));
#26036=CARTESIAN_POINT('Ctrl Pts',(0.607711315454876,1.,2.1074919961518));
#26037=CARTESIAN_POINT('Ctrl Pts',(0.610560911689898,1.,2.11012443807238));
#26038=CARTESIAN_POINT('Ctrl Pts',(0.6124673655618,1.,2.11187554259986));
#26039=CARTESIAN_POINT('Ctrl Pts',(0.61342227326009,1.,2.11275013067528));
#26040=CARTESIAN_POINT('',(0.383122945602003,0.,1.7075470150345));
#26041=CARTESIAN_POINT('Origin',(0.,0.,0.));
#26042=CARTESIAN_POINT('',(0.163289472382896,1.,1.74236521665491));
#26043=CARTESIAN_POINT('Origin',(0.,1.,0.));
#26044=CARTESIAN_POINT('',(0.163289472382896,0.,1.74236521665491));
#26045=CARTESIAN_POINT('Ctrl Pts',(0.0694764450219578,-1.,2.19890268624765));
#26046=CARTESIAN_POINT('Ctrl Pts',(0.0694764450219578,1.,2.19890268624765));
#26047=CARTESIAN_POINT('Ctrl Pts',(0.0701143536325487,-1.,2.19777582085423));
#26048=CARTESIAN_POINT('Ctrl Pts',(0.0701143536325487,1.,2.19777582085423));
#26049=CARTESIAN_POINT('Ctrl Pts',(0.0713863779526151,-1.,2.19552129484002));
#26050=CARTESIAN_POINT('Ctrl Pts',(0.0713863779526151,1.,2.19552129484002));
#26051=CARTESIAN_POINT('Ctrl Pts',(0.0732830357306722,-1.,2.19213712013662));
#26052=CARTESIAN_POINT('Ctrl Pts',(0.0732830357306722,1.,2.19213712013662));
#26053=CARTESIAN_POINT('Ctrl Pts',(0.0757891465836145,-1.,2.1876201139953));
#26054=CARTESIAN_POINT('Ctrl Pts',(0.0757891465836145,1.,2.1876201139953));
#26055=CARTESIAN_POINT('Ctrl Pts',(0.078883772768524,-1.,2.18196589448887));
#26056=CARTESIAN_POINT('Ctrl Pts',(0.078883772768524,1.,2.18196589448887));
#26057=CARTESIAN_POINT('Ctrl Pts',(0.0819402680872763,-1.,2.176303712113));
#26058=CARTESIAN_POINT('Ctrl Pts',(0.0819402680872763,1.,2.176303712113));
#26059=CARTESIAN_POINT('Ctrl Pts',(0.084958462083537,-1.,2.17063357870952));
#26060=CARTESIAN_POINT('Ctrl Pts',(0.084958462083537,1.,2.17063357870952));
#26061=CARTESIAN_POINT('Ctrl Pts',(0.087938129138692,-1.,2.16495552645014));
#26062=CARTESIAN_POINT('Ctrl Pts',(0.087938129138692,1.,2.16495552645014));
#26063=CARTESIAN_POINT('Ctrl Pts',(0.0908789888107263,-1.,2.15926961544516));
#26064=CARTESIAN_POINT('Ctrl Pts',(0.0908789888107263,1.,2.15926961544516));
#26065=CARTESIAN_POINT('Ctrl Pts',(0.0937807218867641,-1.,2.1535759397817));
#26066=CARTESIAN_POINT('Ctrl Pts',(0.0937807218867641,1.,2.1535759397817));
#26067=CARTESIAN_POINT('Ctrl Pts',(0.0966429852305456,-1.,2.14787463531795));
#26068=CARTESIAN_POINT('Ctrl Pts',(0.0966429852305456,1.,2.14787463531795));
#26069=CARTESIAN_POINT('Ctrl Pts',(0.0994654261990913,-1.,2.14216588396025));
#26070=CARTESIAN_POINT('Ctrl Pts',(0.0994654261990913,1.,2.14216588396025));
#26071=CARTESIAN_POINT('Ctrl Pts',(0.1022477005561,-1.,2.13644992667165));
#26072=CARTESIAN_POINT('Ctrl Pts',(0.1022477005561,1.,2.13644992667165));
#26073=CARTESIAN_POINT('Ctrl Pts',(0.104989479152739,-1.,2.13072704887293));
#26074=CARTESIAN_POINT('Ctrl Pts',(0.104989479152739,1.,2.13072704887293));
#26075=CARTESIAN_POINT('Ctrl Pts',(0.10769043523109,-1.,2.12499752307));
#26076=CARTESIAN_POINT('Ctrl Pts',(0.10769043523109,1.,2.12499752307));
#26077=CARTESIAN_POINT('Ctrl Pts',(0.110350236135025,-1.,2.11926155590865));
#26078=CARTESIAN_POINT('Ctrl Pts',(0.110350236135025,1.,2.11926155590865));
#26079=CARTESIAN_POINT('Ctrl Pts',(0.112968534419737,-1.,2.11351924490306));
#26080=CARTESIAN_POINT('Ctrl Pts',(0.112968534419737,1.,2.11351924490306));
#26081=CARTESIAN_POINT('Ctrl Pts',(0.115544957687926,-1.,2.10777050261309));
#26082=CARTESIAN_POINT('Ctrl Pts',(0.115544957687926,1.,2.10777050261309));
#26083=CARTESIAN_POINT('Ctrl Pts',(0.118079107988355,-1.,2.102015121329));
#26084=CARTESIAN_POINT('Ctrl Pts',(0.118079107988355,1.,2.102015121329));
#26085=CARTESIAN_POINT('Ctrl Pts',(0.120570567965122,-1.,2.0962529286773));
#26086=CARTESIAN_POINT('Ctrl Pts',(0.120570567965122,1.,2.0962529286773));
#26087=CARTESIAN_POINT('Ctrl Pts',(0.123018905621083,-1.,2.09048392424825));
#26088=CARTESIAN_POINT('Ctrl Pts',(0.123018905621083,1.,2.09048392424825));
#26089=CARTESIAN_POINT('Ctrl Pts',(0.125423679412061,-1.,2.08470840653643));
#26090=CARTESIAN_POINT('Ctrl Pts',(0.125423679412061,1.,2.08470840653643));
#26091=CARTESIAN_POINT('Ctrl Pts',(0.12778444527612,-1.,2.07892715110987));
#26092=CARTESIAN_POINT('Ctrl Pts',(0.12778444527612,1.,2.07892715110987));
#26093=CARTESIAN_POINT('Ctrl Pts',(0.130100748328403,-1.,2.07314114713063));
#26094=CARTESIAN_POINT('Ctrl Pts',(0.130100748328403,1.,2.07314114713063));
#26095=CARTESIAN_POINT('Ctrl Pts',(0.13237211154771,-1.,2.06735123910326));
#26096=CARTESIAN_POINT('Ctrl Pts',(0.13237211154771,1.,2.06735123910326));
#26097=CARTESIAN_POINT('Ctrl Pts',(0.134598026192106,-1.,2.06155781517842));
#26098=CARTESIAN_POINT('Ctrl Pts',(0.134598026192106,1.,2.06155781517842));
#26099=CARTESIAN_POINT('Ctrl Pts',(0.136777941218043,-1.,2.05576044414264));
#26100=CARTESIAN_POINT('Ctrl Pts',(0.136777941218043,1.,2.05576044414264));
#26101=CARTESIAN_POINT('Ctrl Pts',(0.138911255368966,-1.,2.04995762001328));
#26102=CARTESIAN_POINT('Ctrl Pts',(0.138911255368966,1.,2.04995762001328));
#26103=CARTESIAN_POINT('Ctrl Pts',(0.140997332152546,-1.,2.04414757947916));
#26104=CARTESIAN_POINT('Ctrl Pts',(0.140997332152546,1.,2.04414757947916));
#26105=CARTESIAN_POINT('Ctrl Pts',(0.143035515058208,-1.,2.03832911025912));
#26106=CARTESIAN_POINT('Ctrl Pts',(0.143035515058208,1.,2.03832911025912));
#26107=CARTESIAN_POINT('Ctrl Pts',(0.145025140186057,-1.,2.03250223739942));
#26108=CARTESIAN_POINT('Ctrl Pts',(0.145025140186057,1.,2.03250223739942));
#26109=CARTESIAN_POINT('Ctrl Pts',(0.146965557332583,-1.,2.02666926182017));
#26110=CARTESIAN_POINT('Ctrl Pts',(0.146965557332583,1.,2.02666926182017));
#26111=CARTESIAN_POINT('Ctrl Pts',(0.148856124775337,-1.,2.02083464969894));
#26112=CARTESIAN_POINT('Ctrl Pts',(0.148856124775337,1.,2.02083464969894));
#26113=CARTESIAN_POINT('Ctrl Pts',(0.150696157673078,-1.,2.01500291940238));
#26114=CARTESIAN_POINT('Ctrl Pts',(0.150696157673078,1.,2.01500291940238));
#26115=CARTESIAN_POINT('Ctrl Pts',(0.152484883621449,-1.,2.00917680318424));
#26116=CARTESIAN_POINT('Ctrl Pts',(0.152484883621449,1.,2.00917680318424));
#26117=CARTESIAN_POINT('Ctrl Pts',(0.154221403049722,-1.,2.00335565310543));
#26118=CARTESIAN_POINT('Ctrl Pts',(0.154221403049722,1.,2.00335565310543));
#26119=CARTESIAN_POINT('Ctrl Pts',(0.155904629548783,-1.,1.99753284771497));
#26120=CARTESIAN_POINT('Ctrl Pts',(0.155904629548783,1.,1.99753284771497));
#26121=CARTESIAN_POINT('Ctrl Pts',(0.157533331459227,-1.,1.99169810931908));
#26122=CARTESIAN_POINT('Ctrl Pts',(0.157533331459227,1.,1.99169810931908));
#26123=CARTESIAN_POINT('Ctrl Pts',(0.159106226437299,-1.,1.98584238283292));
#26124=CARTESIAN_POINT('Ctrl Pts',(0.159106226437299,1.,1.98584238283292));
#26125=CARTESIAN_POINT('Ctrl Pts',(0.160622060784611,-1.,1.97996195437559));
#26126=CARTESIAN_POINT('Ctrl Pts',(0.160622060784611,1.,1.97996195437559));
#26127=CARTESIAN_POINT('Ctrl Pts',(0.162079693556288,-1.,1.97406280235188));
#26128=CARTESIAN_POINT('Ctrl Pts',(0.162079693556288,1.,1.97406280235188));
#26129=CARTESIAN_POINT('Ctrl Pts',(0.163478185457734,-1.,1.96816512677967));
#26130=CARTESIAN_POINT('Ctrl Pts',(0.163478185457734,1.,1.96816512677967));
#26131=CARTESIAN_POINT('Ctrl Pts',(0.164816568920269,-1.,1.96229379940136));
#26132=CARTESIAN_POINT('Ctrl Pts',(0.164816568920269,1.,1.96229379940136));
#26133=CARTESIAN_POINT('Ctrl Pts',(0.166093592002812,-1.,1.9564675971873));
#26134=CARTESIAN_POINT('Ctrl Pts',(0.166093592002812,1.,1.9564675971873));
#26135=CARTESIAN_POINT('Ctrl Pts',(0.167307501784475,-1.,1.95069027794294));
#26136=CARTESIAN_POINT('Ctrl Pts',(0.167307501784475,1.,1.95069027794294));
#26137=CARTESIAN_POINT('Ctrl Pts',(0.168455741607556,-1.,1.94493757756931));
#26138=CARTESIAN_POINT('Ctrl Pts',(0.168455741607556,1.,1.94493757756931));
#26139=CARTESIAN_POINT('Ctrl Pts',(0.16953490481749,-1.,1.93915639211581));
#26140=CARTESIAN_POINT('Ctrl Pts',(0.16953490481749,1.,1.93915639211581));
#26141=CARTESIAN_POINT('Ctrl Pts',(0.170541253116201,-1.,1.93329183155539));
#26142=CARTESIAN_POINT('Ctrl Pts',(0.170541253116201,1.,1.93329183155539));
#26143=CARTESIAN_POINT('Ctrl Pts',(0.171471191532988,-1.,1.92731093582036));
#26144=CARTESIAN_POINT('Ctrl Pts',(0.171471191532988,1.,1.92731093582036));
#26145=CARTESIAN_POINT('Ctrl Pts',(0.172321621259513,-1.,1.9212233439798));
#26146=CARTESIAN_POINT('Ctrl Pts',(0.172321621259513,1.,1.9212233439798));
#26147=CARTESIAN_POINT('Ctrl Pts',(0.173090695383496,-1.,1.91511429159527));
#26148=CARTESIAN_POINT('Ctrl Pts',(0.173090695383496,1.,1.91511429159527));
#26149=CARTESIAN_POINT('Ctrl Pts',(0.173776635257816,-1.,1.90911693975267));
#26150=CARTESIAN_POINT('Ctrl Pts',(0.173776635257816,1.,1.90911693975267));
#26151=CARTESIAN_POINT('Ctrl Pts',(0.174375518661085,-1.,1.90335253862834));
#26152=CARTESIAN_POINT('Ctrl Pts',(0.174375518661085,1.,1.90335253862834));
#26153=CARTESIAN_POINT('Ctrl Pts',(0.174879405091263,-1.,1.89788101117132));
#26154=CARTESIAN_POINT('Ctrl Pts',(0.174879405091263,1.,1.89788101117132));
#26155=CARTESIAN_POINT('Ctrl Pts',(0.175274276190844,-1.,1.892646301985));
#26156=CARTESIAN_POINT('Ctrl Pts',(0.175274276190844,1.,1.892646301985));
#26157=CARTESIAN_POINT('Ctrl Pts',(0.175538155840648,-1.,1.88742606273259));
#26158=CARTESIAN_POINT('Ctrl Pts',(0.175538155840648,1.,1.88742606273259));
#26159=CARTESIAN_POINT('Ctrl Pts',(0.175644148889698,-1.,1.88188663145367));
#26160=CARTESIAN_POINT('Ctrl Pts',(0.175644148889698,1.,1.88188663145367));
#26161=CARTESIAN_POINT('Ctrl Pts',(0.175563480746485,-1.,1.87563767773588));
#26162=CARTESIAN_POINT('Ctrl Pts',(0.175563480746485,1.,1.87563767773588));
#26163=CARTESIAN_POINT('Ctrl Pts',(0.175268337590757,-1.,1.86828349694799));
#26164=CARTESIAN_POINT('Ctrl Pts',(0.175268337590757,1.,1.86828349694799));
#26165=CARTESIAN_POINT('Ctrl Pts',(0.17473525927603,-1.,1.85948367088837));
#26166=CARTESIAN_POINT('Ctrl Pts',(0.17473525927603,1.,1.85948367088837));
#26167=CARTESIAN_POINT('Ctrl Pts',(0.173946627587731,-1.,1.8489811319852));
#26168=CARTESIAN_POINT('Ctrl Pts',(0.173946627587731,1.,1.8489811319852));
#26169=CARTESIAN_POINT('Ctrl Pts',(0.1728894428919,-1.,1.83658380527692));
#26170=CARTESIAN_POINT('Ctrl Pts',(0.1728894428919,1.,1.83658380527692));
#26171=CARTESIAN_POINT('Ctrl Pts',(0.171554770204119,-1.,1.82215766811545));
#26172=CARTESIAN_POINT('Ctrl Pts',(0.171554770204119,1.,1.82215766811545));
#26173=CARTESIAN_POINT('Ctrl Pts',(0.169936923904608,-1.,1.80561530629706));
#26174=CARTESIAN_POINT('Ctrl Pts',(0.169936923904608,1.,1.80561530629706));
#26175=CARTESIAN_POINT('Ctrl Pts',(0.168032772805197,-1.,1.7869064998507));
#26176=CARTESIAN_POINT('Ctrl Pts',(0.168032772805197,1.,1.7869064998507));
#26177=CARTESIAN_POINT('Ctrl Pts',(0.1662793551464,-1.,1.77018771684844));
#26178=CARTESIAN_POINT('Ctrl Pts',(0.1662793551464,1.,1.77018771684844));
#26179=CARTESIAN_POINT('Ctrl Pts',(0.164834765707158,-1.,1.75666056638427));
#26180=CARTESIAN_POINT('Ctrl Pts',(0.164834765707158,1.,1.75666056638427));
#26181=CARTESIAN_POINT('Ctrl Pts',(0.163814161002002,-1.,1.7472034950333));
#26182=CARTESIAN_POINT('Ctrl Pts',(0.163814161002002,1.,1.7472034950333));
#26183=CARTESIAN_POINT('Ctrl Pts',(0.163289472382896,-1.,1.74236521665491));
#26184=CARTESIAN_POINT('Ctrl Pts',(0.163289472382896,1.,1.74236521665491));
#26185=CARTESIAN_POINT('',(0.0694764450219578,1.,2.19890268624765));
#26186=CARTESIAN_POINT('Ctrl Pts',(0.0694764450219578,1.,2.19890268624765));
#26187=CARTESIAN_POINT('Ctrl Pts',(0.0701143536325487,1.,2.19777582085423));
#26188=CARTESIAN_POINT('Ctrl Pts',(0.0713863779526151,1.,2.19552129484002));
#26189=CARTESIAN_POINT('Ctrl Pts',(0.0732830357306722,1.,2.19213712013662));
#26190=CARTESIAN_POINT('Ctrl Pts',(0.0757891465836145,1.,2.1876201139953));
#26191=CARTESIAN_POINT('Ctrl Pts',(0.078883772768524,1.,2.18196589448887));
#26192=CARTESIAN_POINT('Ctrl Pts',(0.0819402680872763,1.,2.176303712113));
#26193=CARTESIAN_POINT('Ctrl Pts',(0.084958462083537,1.,2.17063357870952));
#26194=CARTESIAN_POINT('Ctrl Pts',(0.087938129138692,1.,2.16495552645014));
#26195=CARTESIAN_POINT('Ctrl Pts',(0.0908789888107263,1.,2.15926961544516));
#26196=CARTESIAN_POINT('Ctrl Pts',(0.0937807218867641,1.,2.1535759397817));
#26197=CARTESIAN_POINT('Ctrl Pts',(0.0966429852305456,1.,2.14787463531795));
#26198=CARTESIAN_POINT('Ctrl Pts',(0.0994654261990913,1.,2.14216588396025));
#26199=CARTESIAN_POINT('Ctrl Pts',(0.1022477005561,1.,2.13644992667165));
#26200=CARTESIAN_POINT('Ctrl Pts',(0.104989479152739,1.,2.13072704887293));
#26201=CARTESIAN_POINT('Ctrl Pts',(0.10769043523109,1.,2.12499752307));
#26202=CARTESIAN_POINT('Ctrl Pts',(0.110350236135025,1.,2.11926155590865));
#26203=CARTESIAN_POINT('Ctrl Pts',(0.112968534419737,1.,2.11351924490306));
#26204=CARTESIAN_POINT('Ctrl Pts',(0.115544957687926,1.,2.10777050261309));
#26205=CARTESIAN_POINT('Ctrl Pts',(0.118079107988355,1.,2.102015121329));
#26206=CARTESIAN_POINT('Ctrl Pts',(0.120570567965122,1.,2.0962529286773));
#26207=CARTESIAN_POINT('Ctrl Pts',(0.123018905621083,1.,2.09048392424825));
#26208=CARTESIAN_POINT('Ctrl Pts',(0.125423679412061,1.,2.08470840653643));
#26209=CARTESIAN_POINT('Ctrl Pts',(0.12778444527612,1.,2.07892715110987));
#26210=CARTESIAN_POINT('Ctrl Pts',(0.130100748328403,1.,2.07314114713063));
#26211=CARTESIAN_POINT('Ctrl Pts',(0.13237211154771,1.,2.06735123910326));
#26212=CARTESIAN_POINT('Ctrl Pts',(0.134598026192106,1.,2.06155781517842));
#26213=CARTESIAN_POINT('Ctrl Pts',(0.136777941218043,1.,2.05576044414264));
#26214=CARTESIAN_POINT('Ctrl Pts',(0.138911255368966,1.,2.04995762001328));
#26215=CARTESIAN_POINT('Ctrl Pts',(0.140997332152546,1.,2.04414757947916));
#26216=CARTESIAN_POINT('Ctrl Pts',(0.143035515058208,1.,2.03832911025912));
#26217=CARTESIAN_POINT('Ctrl Pts',(0.145025140186057,1.,2.03250223739942));
#26218=CARTESIAN_POINT('Ctrl Pts',(0.146965557332583,1.,2.02666926182017));
#26219=CARTESIAN_POINT('Ctrl Pts',(0.148856124775337,1.,2.02083464969894));
#26220=CARTESIAN_POINT('Ctrl Pts',(0.150696157673078,1.,2.01500291940238));
#26221=CARTESIAN_POINT('Ctrl Pts',(0.152484883621449,1.,2.00917680318424));
#26222=CARTESIAN_POINT('Ctrl Pts',(0.154221403049722,1.,2.00335565310543));
#26223=CARTESIAN_POINT('Ctrl Pts',(0.155904629548783,1.,1.99753284771497));
#26224=CARTESIAN_POINT('Ctrl Pts',(0.157533331459227,1.,1.99169810931908));
#26225=CARTESIAN_POINT('Ctrl Pts',(0.159106226437299,1.,1.98584238283292));
#26226=CARTESIAN_POINT('Ctrl Pts',(0.160622060784611,1.,1.97996195437559));
#26227=CARTESIAN_POINT('Ctrl Pts',(0.162079693556288,1.,1.97406280235188));
#26228=CARTESIAN_POINT('Ctrl Pts',(0.163478185457734,1.,1.96816512677967));
#26229=CARTESIAN_POINT('Ctrl Pts',(0.164816568920269,1.,1.96229379940136));
#26230=CARTESIAN_POINT('Ctrl Pts',(0.166093592002812,1.,1.9564675971873));
#26231=CARTESIAN_POINT('Ctrl Pts',(0.167307501784475,1.,1.95069027794294));
#26232=CARTESIAN_POINT('Ctrl Pts',(0.168455741607556,1.,1.94493757756931));
#26233=CARTESIAN_POINT('Ctrl Pts',(0.16953490481749,1.,1.93915639211581));
#26234=CARTESIAN_POINT('Ctrl Pts',(0.170541253116201,1.,1.93329183155539));
#26235=CARTESIAN_POINT('Ctrl Pts',(0.171471191532988,1.,1.92731093582036));
#26236=CARTESIAN_POINT('Ctrl Pts',(0.172321621259513,1.,1.9212233439798));
#26237=CARTESIAN_POINT('Ctrl Pts',(0.173090695383496,1.,1.91511429159527));
#26238=CARTESIAN_POINT('Ctrl Pts',(0.173776635257816,1.,1.90911693975267));
#26239=CARTESIAN_POINT('Ctrl Pts',(0.174375518661085,1.,1.90335253862834));
#26240=CARTESIAN_POINT('Ctrl Pts',(0.174879405091263,1.,1.89788101117132));
#26241=CARTESIAN_POINT('Ctrl Pts',(0.175274276190844,1.,1.892646301985));
#26242=CARTESIAN_POINT('Ctrl Pts',(0.175538155840648,1.,1.88742606273259));
#26243=CARTESIAN_POINT('Ctrl Pts',(0.175644148889698,1.,1.88188663145367));
#26244=CARTESIAN_POINT('Ctrl Pts',(0.175563480746485,1.,1.87563767773588));
#26245=CARTESIAN_POINT('Ctrl Pts',(0.175268337590757,1.,1.86828349694799));
#26246=CARTESIAN_POINT('Ctrl Pts',(0.17473525927603,1.,1.85948367088837));
#26247=CARTESIAN_POINT('Ctrl Pts',(0.173946627587731,1.,1.8489811319852));
#26248=CARTESIAN_POINT('Ctrl Pts',(0.1728894428919,1.,1.83658380527692));
#26249=CARTESIAN_POINT('Ctrl Pts',(0.171554770204119,1.,1.82215766811545));
#26250=CARTESIAN_POINT('Ctrl Pts',(0.169936923904608,1.,1.80561530629706));
#26251=CARTESIAN_POINT('Ctrl Pts',(0.168032772805197,1.,1.7869064998507));
#26252=CARTESIAN_POINT('Ctrl Pts',(0.1662793551464,1.,1.77018771684844));
#26253=CARTESIAN_POINT('Ctrl Pts',(0.164834765707158,1.,1.75666056638427));
#26254=CARTESIAN_POINT('Ctrl Pts',(0.163814161002002,1.,1.7472034950333));
#26255=CARTESIAN_POINT('Ctrl Pts',(0.163289472382896,1.,1.74236521665491));
#26256=CARTESIAN_POINT('',(0.0694764450219578,0.,2.19890268624765));
#26257=CARTESIAN_POINT('Origin',(-0.0694764450219586,0.,2.19890268624765));
#26258=CARTESIAN_POINT('',(-0.0694764450219586,1.,2.19890268624765));
#26259=CARTESIAN_POINT('',(0.0694764450219578,1.,2.19890268624765));
#26260=CARTESIAN_POINT('',(-0.0694764450219586,0.,2.19890268624765));
#26261=CARTESIAN_POINT('Ctrl Pts',(-0.163289472382896,-1.,1.74236521665491));
#26262=CARTESIAN_POINT('Ctrl Pts',(-0.163289472382896,1.,1.74236521665491));
#26263=CARTESIAN_POINT('Ctrl Pts',(-0.163814161002474,-1.,1.74720349503904));
#26264=CARTESIAN_POINT('Ctrl Pts',(-0.163814161002474,1.,1.74720349503904));
#26265=CARTESIAN_POINT('Ctrl Pts',(-0.164834765708484,-1.,1.75666056640041));
#26266=CARTESIAN_POINT('Ctrl Pts',(-0.164834765708484,1.,1.75666056640041));
#26267=CARTESIAN_POINT('Ctrl Pts',(-0.166279355148738,-1.,1.77018771687692));
#26268=CARTESIAN_POINT('Ctrl Pts',(-0.166279355148738,1.,1.77018771687692));
#26269=CARTESIAN_POINT('Ctrl Pts',(-0.16803277280837,-1.,1.78690649988931));
#26270=CARTESIAN_POINT('Ctrl Pts',(-0.16803277280837,1.,1.78690649988931));
#26271=CARTESIAN_POINT('Ctrl Pts',(-0.169936923908078,-1.,1.80561530633924));
#26272=CARTESIAN_POINT('Ctrl Pts',(-0.169936923908078,1.,1.80561530633924));
#26273=CARTESIAN_POINT('Ctrl Pts',(-0.171554770207306,-1.,1.82215766815414));
#26274=CARTESIAN_POINT('Ctrl Pts',(-0.171554770207306,1.,1.82215766815414));
#26275=CARTESIAN_POINT('Ctrl Pts',(-0.17288944289442,-1.,1.83658380530747));
#26276=CARTESIAN_POINT('Ctrl Pts',(-0.17288944289442,1.,1.83658380530747));
#26277=CARTESIAN_POINT('Ctrl Pts',(-0.173946627589401,-1.,1.84898113200543));
#26278=CARTESIAN_POINT('Ctrl Pts',(-0.173946627589401,1.,1.84898113200543));
#26279=CARTESIAN_POINT('Ctrl Pts',(-0.174735259276856,-1.,1.85948367089838));
#26280=CARTESIAN_POINT('Ctrl Pts',(-0.174735259276856,1.,1.85948367089838));
#26281=CARTESIAN_POINT('Ctrl Pts',(-0.175268337590901,-1.,1.86828349694972));
#26282=CARTESIAN_POINT('Ctrl Pts',(-0.175268337590901,1.,1.86828349694972));
#26283=CARTESIAN_POINT('Ctrl Pts',(-0.175563480746206,-1.,1.87563767773249));
#26284=CARTESIAN_POINT('Ctrl Pts',(-0.175563480746206,1.,1.87563767773249));
#26285=CARTESIAN_POINT('Ctrl Pts',(-0.175644148889271,-1.,1.88188663144846));
#26286=CARTESIAN_POINT('Ctrl Pts',(-0.175644148889271,1.,1.88188663144846));
#26287=CARTESIAN_POINT('Ctrl Pts',(-0.175538155840286,-1.,1.88742606272818));
#26288=CARTESIAN_POINT('Ctrl Pts',(-0.175538155840286,1.,1.88742606272818));
#26289=CARTESIAN_POINT('Ctrl Pts',(-0.175274276190664,-1.,1.89264630198279));
#26290=CARTESIAN_POINT('Ctrl Pts',(-0.175274276190664,1.,1.89264630198279));
#26291=CARTESIAN_POINT('Ctrl Pts',(-0.174879405091277,-1.,1.89788101117148));
#26292=CARTESIAN_POINT('Ctrl Pts',(-0.174879405091277,1.,1.89788101117148));
#26293=CARTESIAN_POINT('Ctrl Pts',(-0.174375518661222,-1.,1.90335253863003));
#26294=CARTESIAN_POINT('Ctrl Pts',(-0.174375518661222,1.,1.90335253863003));
#26295=CARTESIAN_POINT('Ctrl Pts',(-0.173776635257984,-1.,1.90911693975475));
#26296=CARTESIAN_POINT('Ctrl Pts',(-0.173776635257984,1.,1.90911693975475));
#26297=CARTESIAN_POINT('Ctrl Pts',(-0.173090695383619,-1.,1.91511429159681));
#26298=CARTESIAN_POINT('Ctrl Pts',(-0.173090695383619,1.,1.91511429159681));
#26299=CARTESIAN_POINT('Ctrl Pts',(-0.172321621259557,-1.,1.92122334398034));
#26300=CARTESIAN_POINT('Ctrl Pts',(-0.172321621259557,1.,1.92122334398034));
#26301=CARTESIAN_POINT('Ctrl Pts',(-0.17147119153296,-1.,1.92731093582));
#26302=CARTESIAN_POINT('Ctrl Pts',(-0.17147119153296,1.,1.92731093582));
#26303=CARTESIAN_POINT('Ctrl Pts',(-0.170541253116136,-1.,1.93329183155455));
#26304=CARTESIAN_POINT('Ctrl Pts',(-0.170541253116136,1.,1.93329183155455));
#26305=CARTESIAN_POINT('Ctrl Pts',(-0.169534904817425,-1.,1.93915639211497));
#26306=CARTESIAN_POINT('Ctrl Pts',(-0.169534904817425,1.,1.93915639211497));
#26307=CARTESIAN_POINT('Ctrl Pts',(-0.168455741607516,-1.,1.94493757756879));
#26308=CARTESIAN_POINT('Ctrl Pts',(-0.168455741607516,1.,1.94493757756879));
#26309=CARTESIAN_POINT('Ctrl Pts',(-0.167307501784469,-1.,1.95069027794286));
#26310=CARTESIAN_POINT('Ctrl Pts',(-0.167307501784469,1.,1.95069027794286));
#26311=CARTESIAN_POINT('Ctrl Pts',(-0.166093592002833,-1.,1.95646759718755));
#26312=CARTESIAN_POINT('Ctrl Pts',(-0.166093592002833,1.,1.95646759718755));
#26313=CARTESIAN_POINT('Ctrl Pts',(-0.1648165689203,-1.,1.96229379940174));
#26314=CARTESIAN_POINT('Ctrl Pts',(-0.1648165689203,1.,1.96229379940174));
#26315=CARTESIAN_POINT('Ctrl Pts',(-0.16347818545776,-1.,1.96816512678));
#26316=CARTESIAN_POINT('Ctrl Pts',(-0.16347818545776,1.,1.96816512678));
#26317=CARTESIAN_POINT('Ctrl Pts',(-0.162079693556302,-1.,1.97406280235204));
#26318=CARTESIAN_POINT('Ctrl Pts',(-0.162079693556302,1.,1.97406280235204));
#26319=CARTESIAN_POINT('Ctrl Pts',(-0.16062206078461,-1.,1.97996195437557));
#26320=CARTESIAN_POINT('Ctrl Pts',(-0.16062206078461,1.,1.97996195437557));
#26321=CARTESIAN_POINT('Ctrl Pts',(-0.159106226437289,-1.,1.98584238283279));
#26322=CARTESIAN_POINT('Ctrl Pts',(-0.159106226437289,1.,1.98584238283279));
#26323=CARTESIAN_POINT('Ctrl Pts',(-0.157533331459215,-1.,1.99169810931893));
#26324=CARTESIAN_POINT('Ctrl Pts',(-0.157533331459215,1.,1.99169810931893));
#26325=CARTESIAN_POINT('Ctrl Pts',(-0.155904629548775,-1.,1.99753284771487));
#26326=CARTESIAN_POINT('Ctrl Pts',(-0.155904629548775,1.,1.99753284771487));
#26327=CARTESIAN_POINT('Ctrl Pts',(-0.154221403049719,-1.,2.00335565310539));
#26328=CARTESIAN_POINT('Ctrl Pts',(-0.154221403049719,1.,2.00335565310539));
#26329=CARTESIAN_POINT('Ctrl Pts',(-0.152484883621452,-1.,2.00917680318426));
#26330=CARTESIAN_POINT('Ctrl Pts',(-0.152484883621452,1.,2.00917680318426));
#26331=CARTESIAN_POINT('Ctrl Pts',(-0.150696157673084,-1.,2.01500291940243));
#26332=CARTESIAN_POINT('Ctrl Pts',(-0.150696157673084,1.,2.01500291940243));
#26333=CARTESIAN_POINT('Ctrl Pts',(-0.148856124775343,-1.,2.02083464969897));
#26334=CARTESIAN_POINT('Ctrl Pts',(-0.148856124775343,1.,2.02083464969897));
#26335=CARTESIAN_POINT('Ctrl Pts',(-0.146965557332586,-1.,2.02666926182017));
#26336=CARTESIAN_POINT('Ctrl Pts',(-0.146965557332586,1.,2.02666926182017));
#26337=CARTESIAN_POINT('Ctrl Pts',(-0.145025140186058,-1.,2.03250223739941));
#26338=CARTESIAN_POINT('Ctrl Pts',(-0.145025140186058,1.,2.03250223739941));
#26339=CARTESIAN_POINT('Ctrl Pts',(-0.143035515058208,-1.,2.03832911025913));
#26340=CARTESIAN_POINT('Ctrl Pts',(-0.143035515058208,1.,2.03832911025913));
#26341=CARTESIAN_POINT('Ctrl Pts',(-0.140997332152546,-1.,2.04414757947919));
#26342=CARTESIAN_POINT('Ctrl Pts',(-0.140997332152546,1.,2.04414757947919));
#26343=CARTESIAN_POINT('Ctrl Pts',(-0.138911255368966,-1.,2.04995762001333));
#26344=CARTESIAN_POINT('Ctrl Pts',(-0.138911255368966,1.,2.04995762001333));
#26345=CARTESIAN_POINT('Ctrl Pts',(-0.136777941218044,-1.,2.0557604441427));
#26346=CARTESIAN_POINT('Ctrl Pts',(-0.136777941218044,1.,2.0557604441427));
#26347=CARTESIAN_POINT('Ctrl Pts',(-0.134598026192107,-1.,2.06155781517844));
#26348=CARTESIAN_POINT('Ctrl Pts',(-0.134598026192107,1.,2.06155781517844));
#26349=CARTESIAN_POINT('Ctrl Pts',(-0.13237211154771,-1.,2.06735123910319));
#26350=CARTESIAN_POINT('Ctrl Pts',(-0.13237211154771,1.,2.06735123910319));
#26351=CARTESIAN_POINT('Ctrl Pts',(-0.130100748328401,-1.,2.07314114713047));
#26352=CARTESIAN_POINT('Ctrl Pts',(-0.130100748328401,1.,2.07314114713047));
#26353=CARTESIAN_POINT('Ctrl Pts',(-0.127784445276116,-1.,2.07892715110967));
#26354=CARTESIAN_POINT('Ctrl Pts',(-0.127784445276116,1.,2.07892715110967));
#26355=CARTESIAN_POINT('Ctrl Pts',(-0.125423679412058,-1.,2.08470840653628));
#26356=CARTESIAN_POINT('Ctrl Pts',(-0.125423679412058,1.,2.08470840653628));
#26357=CARTESIAN_POINT('Ctrl Pts',(-0.123018905621083,-1.,2.09048392424826));
#26358=CARTESIAN_POINT('Ctrl Pts',(-0.123018905621083,1.,2.09048392424826));
#26359=CARTESIAN_POINT('Ctrl Pts',(-0.120570567965129,-1.,2.09625292867756));
#26360=CARTESIAN_POINT('Ctrl Pts',(-0.120570567965129,1.,2.09625292867756));
#26361=CARTESIAN_POINT('Ctrl Pts',(-0.118079107988368,-1.,2.10201512132945));
#26362=CARTESIAN_POINT('Ctrl Pts',(-0.118079107988368,1.,2.10201512132945));
#26363=CARTESIAN_POINT('Ctrl Pts',(-0.115544957687941,-1.,2.10777050261359));
#26364=CARTESIAN_POINT('Ctrl Pts',(-0.115544957687941,1.,2.10777050261359));
#26365=CARTESIAN_POINT('Ctrl Pts',(-0.112968534419746,-1.,2.11351924490335));
#26366=CARTESIAN_POINT('Ctrl Pts',(-0.112968534419746,1.,2.11351924490335));
#26367=CARTESIAN_POINT('Ctrl Pts',(-0.11035023613502,-1.,2.11926155590849));
#26368=CARTESIAN_POINT('Ctrl Pts',(-0.11035023613502,1.,2.11926155590849));
#26369=CARTESIAN_POINT('Ctrl Pts',(-0.107690435231068,-1.,2.12499752306927));
#26370=CARTESIAN_POINT('Ctrl Pts',(-0.107690435231068,1.,2.12499752306927));
#26371=CARTESIAN_POINT('Ctrl Pts',(-0.104989479152703,-1.,2.1307270488718));
#26372=CARTESIAN_POINT('Ctrl Pts',(-0.104989479152703,1.,2.1307270488718));
#26373=CARTESIAN_POINT('Ctrl Pts',(-0.102247700556064,-1.,2.13644992667052));
#26374=CARTESIAN_POINT('Ctrl Pts',(-0.102247700556064,1.,2.13644992667052));
#26375=CARTESIAN_POINT('Ctrl Pts',(-0.0994654261990745,-1.,2.14216588395974));
#26376=CARTESIAN_POINT('Ctrl Pts',(-0.0994654261990745,1.,2.14216588395974));
#26377=CARTESIAN_POINT('Ctrl Pts',(-0.0966429852305691,-1.,2.14787463531864));
#26378=CARTESIAN_POINT('Ctrl Pts',(-0.0966429852305691,1.,2.14787463531864));
#26379=CARTESIAN_POINT('Ctrl Pts',(-0.0937807218868348,-1.,2.15357593978377));
#26380=CARTESIAN_POINT('Ctrl Pts',(-0.0937807218868348,1.,2.15357593978377));
#26381=CARTESIAN_POINT('Ctrl Pts',(-0.0908789888108269,-1.,2.15926961544808));
#26382=CARTESIAN_POINT('Ctrl Pts',(-0.0908789888108269,1.,2.15926961544808));
#26383=CARTESIAN_POINT('Ctrl Pts',(-0.0879381291387825,-1.,2.16495552645275));
#26384=CARTESIAN_POINT('Ctrl Pts',(-0.0879381291387825,1.,2.16495552645275));
#26385=CARTESIAN_POINT('Ctrl Pts',(-0.0849584620835646,-1.,2.17063357871031));
#26386=CARTESIAN_POINT('Ctrl Pts',(-0.0849584620835646,1.,2.17063357871031));
#26387=CARTESIAN_POINT('Ctrl Pts',(-0.0819402680871942,-1.,2.1763037121106));
#26388=CARTESIAN_POINT('Ctrl Pts',(-0.0819402680871942,1.,2.1763037121106));
#26389=CARTESIAN_POINT('Ctrl Pts',(-0.078883772768323,-1.,2.18196589448304));
#26390=CARTESIAN_POINT('Ctrl Pts',(-0.078883772768323,1.,2.18196589448304));
#26391=CARTESIAN_POINT('Ctrl Pts',(-0.0757891465833414,-1.,2.1876201139874));
#26392=CARTESIAN_POINT('Ctrl Pts',(-0.0757891465833414,1.,2.1876201139874));
#26393=CARTESIAN_POINT('Ctrl Pts',(-0.0732830357304279,-1.,2.19213712012956));
#26394=CARTESIAN_POINT('Ctrl Pts',(-0.0732830357304279,1.,2.19213712012956));
#26395=CARTESIAN_POINT('Ctrl Pts',(-0.071386377952463,-1.,2.19552129483562));
#26396=CARTESIAN_POINT('Ctrl Pts',(-0.071386377952463,1.,2.19552129483562));
#26397=CARTESIAN_POINT('Ctrl Pts',(-0.0701143536324929,-1.,2.19777582085261));
#26398=CARTESIAN_POINT('Ctrl Pts',(-0.0701143536324929,1.,2.19777582085261));
#26399=CARTESIAN_POINT('Ctrl Pts',(-0.0694764450219586,-1.,2.19890268624765));
#26400=CARTESIAN_POINT('Ctrl Pts',(-0.0694764450219586,1.,2.19890268624765));
#26401=CARTESIAN_POINT('',(-0.163289472382896,1.,1.74236521665491));
#26402=CARTESIAN_POINT('Ctrl Pts',(-0.163289472382896,1.,1.74236521665491));
#26403=CARTESIAN_POINT('Ctrl Pts',(-0.163814161002474,1.,1.74720349503904));
#26404=CARTESIAN_POINT('Ctrl Pts',(-0.164834765708484,1.,1.75666056640041));
#26405=CARTESIAN_POINT('Ctrl Pts',(-0.166279355148738,1.,1.77018771687692));
#26406=CARTESIAN_POINT('Ctrl Pts',(-0.16803277280837,1.,1.78690649988931));
#26407=CARTESIAN_POINT('Ctrl Pts',(-0.169936923908078,1.,1.80561530633924));
#26408=CARTESIAN_POINT('Ctrl Pts',(-0.171554770207306,1.,1.82215766815414));
#26409=CARTESIAN_POINT('Ctrl Pts',(-0.17288944289442,1.,1.83658380530747));
#26410=CARTESIAN_POINT('Ctrl Pts',(-0.173946627589401,1.,1.84898113200543));
#26411=CARTESIAN_POINT('Ctrl Pts',(-0.174735259276856,1.,1.85948367089838));
#26412=CARTESIAN_POINT('Ctrl Pts',(-0.175268337590901,1.,1.86828349694972));
#26413=CARTESIAN_POINT('Ctrl Pts',(-0.175563480746206,1.,1.87563767773249));
#26414=CARTESIAN_POINT('Ctrl Pts',(-0.175644148889271,1.,1.88188663144846));
#26415=CARTESIAN_POINT('Ctrl Pts',(-0.175538155840286,1.,1.88742606272818));
#26416=CARTESIAN_POINT('Ctrl Pts',(-0.175274276190664,1.,1.89264630198279));
#26417=CARTESIAN_POINT('Ctrl Pts',(-0.174879405091277,1.,1.89788101117148));
#26418=CARTESIAN_POINT('Ctrl Pts',(-0.174375518661222,1.,1.90335253863003));
#26419=CARTESIAN_POINT('Ctrl Pts',(-0.173776635257984,1.,1.90911693975475));
#26420=CARTESIAN_POINT('Ctrl Pts',(-0.173090695383619,1.,1.91511429159681));
#26421=CARTESIAN_POINT('Ctrl Pts',(-0.172321621259557,1.,1.92122334398034));
#26422=CARTESIAN_POINT('Ctrl Pts',(-0.17147119153296,1.,1.92731093582));
#26423=CARTESIAN_POINT('Ctrl Pts',(-0.170541253116136,1.,1.93329183155455));
#26424=CARTESIAN_POINT('Ctrl Pts',(-0.169534904817425,1.,1.93915639211497));
#26425=CARTESIAN_POINT('Ctrl Pts',(-0.168455741607516,1.,1.94493757756879));
#26426=CARTESIAN_POINT('Ctrl Pts',(-0.167307501784469,1.,1.95069027794286));
#26427=CARTESIAN_POINT('Ctrl Pts',(-0.166093592002833,1.,1.95646759718755));
#26428=CARTESIAN_POINT('Ctrl Pts',(-0.1648165689203,1.,1.96229379940174));
#26429=CARTESIAN_POINT('Ctrl Pts',(-0.16347818545776,1.,1.96816512678));
#26430=CARTESIAN_POINT('Ctrl Pts',(-0.162079693556302,1.,1.97406280235204));
#26431=CARTESIAN_POINT('Ctrl Pts',(-0.16062206078461,1.,1.97996195437557));
#26432=CARTESIAN_POINT('Ctrl Pts',(-0.159106226437289,1.,1.98584238283279));
#26433=CARTESIAN_POINT('Ctrl Pts',(-0.157533331459215,1.,1.99169810931893));
#26434=CARTESIAN_POINT('Ctrl Pts',(-0.155904629548775,1.,1.99753284771487));
#26435=CARTESIAN_POINT('Ctrl Pts',(-0.154221403049719,1.,2.00335565310539));
#26436=CARTESIAN_POINT('Ctrl Pts',(-0.152484883621452,1.,2.00917680318426));
#26437=CARTESIAN_POINT('Ctrl Pts',(-0.150696157673084,1.,2.01500291940243));
#26438=CARTESIAN_POINT('Ctrl Pts',(-0.148856124775343,1.,2.02083464969897));
#26439=CARTESIAN_POINT('Ctrl Pts',(-0.146965557332586,1.,2.02666926182017));
#26440=CARTESIAN_POINT('Ctrl Pts',(-0.145025140186058,1.,2.03250223739941));
#26441=CARTESIAN_POINT('Ctrl Pts',(-0.143035515058208,1.,2.03832911025913));
#26442=CARTESIAN_POINT('Ctrl Pts',(-0.140997332152546,1.,2.04414757947919));
#26443=CARTESIAN_POINT('Ctrl Pts',(-0.138911255368966,1.,2.04995762001333));
#26444=CARTESIAN_POINT('Ctrl Pts',(-0.136777941218044,1.,2.0557604441427));
#26445=CARTESIAN_POINT('Ctrl Pts',(-0.134598026192107,1.,2.06155781517844));
#26446=CARTESIAN_POINT('Ctrl Pts',(-0.13237211154771,1.,2.06735123910319));
#26447=CARTESIAN_POINT('Ctrl Pts',(-0.130100748328401,1.,2.07314114713047));
#26448=CARTESIAN_POINT('Ctrl Pts',(-0.127784445276116,1.,2.07892715110967));
#26449=CARTESIAN_POINT('Ctrl Pts',(-0.125423679412058,1.,2.08470840653628));
#26450=CARTESIAN_POINT('Ctrl Pts',(-0.123018905621083,1.,2.09048392424826));
#26451=CARTESIAN_POINT('Ctrl Pts',(-0.120570567965129,1.,2.09625292867756));
#26452=CARTESIAN_POINT('Ctrl Pts',(-0.118079107988368,1.,2.10201512132945));
#26453=CARTESIAN_POINT('Ctrl Pts',(-0.115544957687941,1.,2.10777050261359));
#26454=CARTESIAN_POINT('Ctrl Pts',(-0.112968534419746,1.,2.11351924490335));
#26455=CARTESIAN_POINT('Ctrl Pts',(-0.11035023613502,1.,2.11926155590849));
#26456=CARTESIAN_POINT('Ctrl Pts',(-0.107690435231068,1.,2.12499752306927));
#26457=CARTESIAN_POINT('Ctrl Pts',(-0.104989479152703,1.,2.1307270488718));
#26458=CARTESIAN_POINT('Ctrl Pts',(-0.102247700556064,1.,2.13644992667052));
#26459=CARTESIAN_POINT('Ctrl Pts',(-0.0994654261990745,1.,2.14216588395974));
#26460=CARTESIAN_POINT('Ctrl Pts',(-0.0966429852305691,1.,2.14787463531864));
#26461=CARTESIAN_POINT('Ctrl Pts',(-0.0937807218868348,1.,2.15357593978377));
#26462=CARTESIAN_POINT('Ctrl Pts',(-0.0908789888108269,1.,2.15926961544808));
#26463=CARTESIAN_POINT('Ctrl Pts',(-0.0879381291387825,1.,2.16495552645275));
#26464=CARTESIAN_POINT('Ctrl Pts',(-0.0849584620835646,1.,2.17063357871031));
#26465=CARTESIAN_POINT('Ctrl Pts',(-0.0819402680871942,1.,2.1763037121106));
#26466=CARTESIAN_POINT('Ctrl Pts',(-0.078883772768323,1.,2.18196589448304));
#26467=CARTESIAN_POINT('Ctrl Pts',(-0.0757891465833414,1.,2.1876201139874));
#26468=CARTESIAN_POINT('Ctrl Pts',(-0.0732830357304279,1.,2.19213712012956));
#26469=CARTESIAN_POINT('Ctrl Pts',(-0.071386377952463,1.,2.19552129483562));
#26470=CARTESIAN_POINT('Ctrl Pts',(-0.0701143536324929,1.,2.19777582085261));
#26471=CARTESIAN_POINT('Ctrl Pts',(-0.0694764450219586,1.,2.19890268624765));
#26472=CARTESIAN_POINT('',(-0.163289472382897,0.,1.74236521665491));
#26473=CARTESIAN_POINT('Origin',(0.,0.,0.));
#26474=CARTESIAN_POINT('',(-0.383122945602004,1.,1.7075470150345));
#26475=CARTESIAN_POINT('Origin',(0.,1.,0.));
#26476=CARTESIAN_POINT('',(-0.383122945602004,0.,1.7075470150345));
#26477=CARTESIAN_POINT('Ctrl Pts',(-0.61342227326009,-1.,2.11275013067528));
#26478=CARTESIAN_POINT('Ctrl Pts',(-0.61342227326009,1.,2.11275013067528));
#26479=CARTESIAN_POINT('Ctrl Pts',(-0.61246736556225,-1.,2.11187554260142));
#26480=CARTESIAN_POINT('Ctrl Pts',(-0.61246736556225,1.,2.11187554260142));
#26481=CARTESIAN_POINT('Ctrl Pts',(-0.610560911691113,-1.,2.11012443807661));
#26482=CARTESIAN_POINT('Ctrl Pts',(-0.610560911691113,1.,2.11012443807661));
#26483=CARTESIAN_POINT('Ctrl Pts',(-0.607711315456826,-1.,2.10749199615859));
#26484=CARTESIAN_POINT('Ctrl Pts',(-0.607711315456826,1.,2.10749199615859));
#26485=CARTESIAN_POINT('Ctrl Pts',(-0.603932030738212,-1.,2.10397049887709));
#26486=CARTESIAN_POINT('Ctrl Pts',(-0.603932030738212,1.,2.10397049887709));
#26487=CARTESIAN_POINT('Ctrl Pts',(-0.599241616422144,-1.,2.09954930865331));
#26488=CARTESIAN_POINT('Ctrl Pts',(-0.599241616422144,1.,2.09954930865331));
#26489=CARTESIAN_POINT('Ctrl Pts',(-0.594585006052824,-1.,2.09510876220501));
#26490=CARTESIAN_POINT('Ctrl Pts',(-0.594585006052824,1.,2.09510876220501));
#26491=CARTESIAN_POINT('Ctrl Pts',(-0.589962365403189,-1.,2.09064881812053));
#26492=CARTESIAN_POINT('Ctrl Pts',(-0.589962365403189,1.,2.09064881812053));
#26493=CARTESIAN_POINT('Ctrl Pts',(-0.585373918990895,-1.,2.086169437277));
#26494=CARTESIAN_POINT('Ctrl Pts',(-0.585373918990895,1.,2.086169437277));
#26495=CARTESIAN_POINT('Ctrl Pts',(-0.580819952107257,-1.,2.08167059018138));
#26496=CARTESIAN_POINT('Ctrl Pts',(-0.580819952107257,1.,2.08167059018138));
#26497=CARTESIAN_POINT('Ctrl Pts',(-0.576300797416275,-1.,2.07715226767361));
#26498=CARTESIAN_POINT('Ctrl Pts',(-0.576300797416275,1.,2.07715226767361));
#26499=CARTESIAN_POINT('Ctrl Pts',(-0.571816823242411,-1.,2.07261449292757));
#26500=CARTESIAN_POINT('Ctrl Pts',(-0.571816823242411,1.,2.07261449292757));
#26501=CARTESIAN_POINT('Ctrl Pts',(-0.567368421181229,-1.,2.06805732997383));
#26502=CARTESIAN_POINT('Ctrl Pts',(-0.567368421181229,1.,2.06805732997383));
#26503=CARTESIAN_POINT('Ctrl Pts',(-0.562955993082574,-1.,2.06348090160697));
#26504=CARTESIAN_POINT('Ctrl Pts',(-0.562955993082574,1.,2.06348090160697));
#26505=CARTESIAN_POINT('Ctrl Pts',(-0.558579940185467,-1.,2.05888537756571));
#26506=CARTESIAN_POINT('Ctrl Pts',(-0.558579940185467,1.,2.05888537756571));
#26507=CARTESIAN_POINT('Ctrl Pts',(-0.55424065746411,-1.,2.05427091604482));
#26508=CARTESIAN_POINT('Ctrl Pts',(-0.55424065746411,1.,2.05427091604482));
#26509=CARTESIAN_POINT('Ctrl Pts',(-0.549938525150342,-1.,2.04963761077974));
#26510=CARTESIAN_POINT('Ctrl Pts',(-0.549938525150342,1.,2.04963761077974));
#26511=CARTESIAN_POINT('Ctrl Pts',(-0.545673903817348,-1.,2.0449854471456));
#26512=CARTESIAN_POINT('Ctrl Pts',(-0.545673903817348,1.,2.0449854471456));
#26513=CARTESIAN_POINT('Ctrl Pts',(-0.54144712061552,-1.,2.0403142269048));
#26514=CARTESIAN_POINT('Ctrl Pts',(-0.54144712061552,1.,2.0403142269048));
#26515=CARTESIAN_POINT('Ctrl Pts',(-0.537258489833134,-1.,2.03562362953993));
#26516=CARTESIAN_POINT('Ctrl Pts',(-0.537258489833134,1.,2.03562362953993));
#26517=CARTESIAN_POINT('Ctrl Pts',(-0.533108355132905,-1.,2.03091336214401));
#26518=CARTESIAN_POINT('Ctrl Pts',(-0.533108355132905,1.,2.03091336214401));
#26519=CARTESIAN_POINT('Ctrl Pts',(-0.528997127241911,-1.,2.02618329083289));
#26520=CARTESIAN_POINT('Ctrl Pts',(-0.528997127241911,1.,2.02618329083289));
#26521=CARTESIAN_POINT('Ctrl Pts',(-0.524925318333518,-1.,2.02143356304712));
#26522=CARTESIAN_POINT('Ctrl Pts',(-0.524925318333518,1.,2.02143356304712));
#26523=CARTESIAN_POINT('Ctrl Pts',(-0.520893590399428,-1.,2.01666477917305));
#26524=CARTESIAN_POINT('Ctrl Pts',(-0.520893590399428,1.,2.01666477917305));
#26525=CARTESIAN_POINT('Ctrl Pts',(-0.516902681728733,-1.,2.01187773939257));
#26526=CARTESIAN_POINT('Ctrl Pts',(-0.516902681728733,1.,2.01187773939257));
#26527=CARTESIAN_POINT('Ctrl Pts',(-0.512953306961814,-1.,2.00707309946955));
#26528=CARTESIAN_POINT('Ctrl Pts',(-0.512953306961814,1.,2.00707309946955));
#26529=CARTESIAN_POINT('Ctrl Pts',(-0.509046069886152,-1.,2.00225107134733));
#26530=CARTESIAN_POINT('Ctrl Pts',(-0.509046069886152,1.,2.00225107134733));
#26531=CARTESIAN_POINT('Ctrl Pts',(-0.505181361323011,-1.,1.99741107463567));
#26532=CARTESIAN_POINT('Ctrl Pts',(-0.505181361323011,1.,1.99741107463567));
#26533=CARTESIAN_POINT('Ctrl Pts',(-0.501359287727129,-1.,1.9925514912615));
#26534=CARTESIAN_POINT('Ctrl Pts',(-0.501359287727129,1.,1.9925514912615));
#26535=CARTESIAN_POINT('Ctrl Pts',(-0.497579909545564,-1.,1.98767044752929));
#26536=CARTESIAN_POINT('Ctrl Pts',(-0.497579909545564,1.,1.98767044752929));
#26537=CARTESIAN_POINT('Ctrl Pts',(-0.493843476541492,-1.,1.9827665876182));
#26538=CARTESIAN_POINT('Ctrl Pts',(-0.493843476541492,1.,1.9827665876182));
#26539=CARTESIAN_POINT('Ctrl Pts',(-0.490150627860955,-1.,1.97783973019229));
#26540=CARTESIAN_POINT('Ctrl Pts',(-0.490150627860955,1.,1.97783973019229));
#26541=CARTESIAN_POINT('Ctrl Pts',(-0.486502692907661,-1.,1.97289186263272));
#26542=CARTESIAN_POINT('Ctrl Pts',(-0.486502692907661,1.,1.97289186263272));
#26543=CARTESIAN_POINT('Ctrl Pts',(-0.482901662120687,-1.,1.96792703422358));
#26544=CARTESIAN_POINT('Ctrl Pts',(-0.482901662120687,1.,1.96792703422358));
#26545=CARTESIAN_POINT('Ctrl Pts',(-0.479349583074846,-1.,1.96294933055938));
#26546=CARTESIAN_POINT('Ctrl Pts',(-0.479349583074846,1.,1.96294933055938));
#26547=CARTESIAN_POINT('Ctrl Pts',(-0.475848034683172,-1.,1.95796111148175));
#26548=CARTESIAN_POINT('Ctrl Pts',(-0.475848034683172,1.,1.95796111148175));
#26549=CARTESIAN_POINT('Ctrl Pts',(-0.47239767226408,-1.,1.95296148278136));
#26550=CARTESIAN_POINT('Ctrl Pts',(-0.47239767226408,1.,1.95296148278136));
#26551=CARTESIAN_POINT('Ctrl Pts',(-0.468997482913158,-1.,1.94794381136524));
#26552=CARTESIAN_POINT('Ctrl Pts',(-0.468997482913158,1.,1.94794381136524));
#26553=CARTESIAN_POINT('Ctrl Pts',(-0.465645462026065,-1.,1.94289794196205));
#26554=CARTESIAN_POINT('Ctrl Pts',(-0.465645462026065,1.,1.94289794196205));
#26555=CARTESIAN_POINT('Ctrl Pts',(-0.462340031009087,-1.,1.93781486640834));
#26556=CARTESIAN_POINT('Ctrl Pts',(-0.462340031009087,1.,1.93781486640834));
#26557=CARTESIAN_POINT('Ctrl Pts',(-0.459081234547931,-1.,1.93269066517936));
#26558=CARTESIAN_POINT('Ctrl Pts',(-0.459081234547931,1.,1.93269066517936));
#26559=CARTESIAN_POINT('Ctrl Pts',(-0.455872005174335,-1.,1.92753067150461));
#26560=CARTESIAN_POINT('Ctrl Pts',(-0.455872005174335,1.,1.92753067150461));
#26561=CARTESIAN_POINT('Ctrl Pts',(-0.452719478359356,-1.,1.9223538064847));
#26562=CARTESIAN_POINT('Ctrl Pts',(-0.452719478359356,1.,1.9223538064847));
#26563=CARTESIAN_POINT('Ctrl Pts',(-0.449632260106572,-1.,1.91718342555717));
#26564=CARTESIAN_POINT('Ctrl Pts',(-0.449632260106572,1.,1.91718342555717));
#26565=CARTESIAN_POINT('Ctrl Pts',(-0.446617343485651,-1.,1.91203699981095));
#26566=CARTESIAN_POINT('Ctrl Pts',(-0.446617343485651,1.,1.91203699981095));
#26567=CARTESIAN_POINT('Ctrl Pts',(-0.44367755684917,-1.,1.90691756144906));
#26568=CARTESIAN_POINT('Ctrl Pts',(-0.44367755684917,1.,1.90691756144906));
#26569=CARTESIAN_POINT('Ctrl Pts',(-0.440807833704161,-1.,1.90180124389137));
#26570=CARTESIAN_POINT('Ctrl Pts',(-0.440807833704161,1.,1.90180124389137));
#26571=CARTESIAN_POINT('Ctrl Pts',(-0.437995003948443,-1.,1.89663648956549));
#26572=CARTESIAN_POINT('Ctrl Pts',(-0.437995003948443,1.,1.89663648956549));
#26573=CARTESIAN_POINT('Ctrl Pts',(-0.43522566096358,-1.,1.89136993975585));
#26574=CARTESIAN_POINT('Ctrl Pts',(-0.43522566096358,1.,1.89136993975585));
#26575=CARTESIAN_POINT('Ctrl Pts',(-0.432493038548833,-1.,1.88596913666828));
#26576=CARTESIAN_POINT('Ctrl Pts',(-0.432493038548833,1.,1.88596913666828));
#26577=CARTESIAN_POINT('Ctrl Pts',(-0.429803062482217,-1.,1.88044229001778));
#26578=CARTESIAN_POINT('Ctrl Pts',(-0.429803062482217,1.,1.88044229001778));
#26579=CARTESIAN_POINT('Ctrl Pts',(-0.427183828518743,-1.,1.87486989291333));
#26580=CARTESIAN_POINT('Ctrl Pts',(-0.427183828518743,1.,1.87486989291333));
#26581=CARTESIAN_POINT('Ctrl Pts',(-0.424678177290876,-1.,1.8693780394412));
#26582=CARTESIAN_POINT('Ctrl Pts',(-0.424678177290876,1.,1.8693780394412));
#26583=CARTESIAN_POINT('Ctrl Pts',(-0.422327307417885,-1.,1.86408083333863));
#26584=CARTESIAN_POINT('Ctrl Pts',(-0.422327307417885,1.,1.86408083333863));
#26585=CARTESIAN_POINT('Ctrl Pts',(-0.420157287975583,-1.,1.8590328109667));
#26586=CARTESIAN_POINT('Ctrl Pts',(-0.420157287975583,1.,1.8590328109667));
#26587=CARTESIAN_POINT('Ctrl Pts',(-0.418164129144045,-1.,1.8541763285645));
#26588=CARTESIAN_POINT('Ctrl Pts',(-0.418164129144045,1.,1.8541763285645));
#26589=CARTESIAN_POINT('Ctrl Pts',(-0.416300022039885,-1.,1.84929312930314));
#26590=CARTESIAN_POINT('Ctrl Pts',(-0.416300022039885,1.,1.84929312930314));
#26591=CARTESIAN_POINT('Ctrl Pts',(-0.414487438255542,-1.,1.84405757074218));
#26592=CARTESIAN_POINT('Ctrl Pts',(-0.414487438255542,1.,1.84405757074218));
#26593=CARTESIAN_POINT('Ctrl Pts',(-0.412633125322945,-1.,1.8380895347617));
#26594=CARTESIAN_POINT('Ctrl Pts',(-0.412633125322945,1.,1.8380895347617));
#26595=CARTESIAN_POINT('Ctrl Pts',(-0.410641256301276,-1.,1.83100408895047));
#26596=CARTESIAN_POINT('Ctrl Pts',(-0.410641256301276,1.,1.83100408895047));
#26597=CARTESIAN_POINT('Ctrl Pts',(-0.408428948106227,-1.,1.82247022677562));
#26598=CARTESIAN_POINT('Ctrl Pts',(-0.408428948106227,1.,1.82247022677562));
#26599=CARTESIAN_POINT('Ctrl Pts',(-0.405933518407175,-1.,1.81223801812013));
#26600=CARTESIAN_POINT('Ctrl Pts',(-0.405933518407175,1.,1.81223801812013));
#26601=CARTESIAN_POINT('Ctrl Pts',(-0.403107976163396,-1.,1.80012077173238));
#26602=CARTESIAN_POINT('Ctrl Pts',(-0.403107976163396,1.,1.80012077173238));
#26603=CARTESIAN_POINT('Ctrl Pts',(-0.399919403774155,-1.,1.78598826343754));
#26604=CARTESIAN_POINT('Ctrl Pts',(-0.399919403774155,1.,1.78598826343754));
#26605=CARTESIAN_POINT('Ctrl Pts',(-0.396346196110688,-1.,1.76975560043442));
#26606=CARTESIAN_POINT('Ctrl Pts',(-0.396346196110688,1.,1.76975560043442));
#26607=CARTESIAN_POINT('Ctrl Pts',(-0.392375812285395,-1.,1.75137405310193));
#26608=CARTESIAN_POINT('Ctrl Pts',(-0.392375812285395,1.,1.75137405310193));
#26609=CARTESIAN_POINT('Ctrl Pts',(-0.388877023502615,-1.,1.73493170972829));
#26610=CARTESIAN_POINT('Ctrl Pts',(-0.388877023502615,1.,1.73493170972829));
#26611=CARTESIAN_POINT('Ctrl Pts',(-0.386070790323281,-1.,1.72162022244582));
#26612=CARTESIAN_POINT('Ctrl Pts',(-0.386070790323281,1.,1.72162022244582));
#26613=CARTESIAN_POINT('Ctrl Pts',(-0.384119047314215,-1.,1.71231062891398));
#26614=CARTESIAN_POINT('Ctrl Pts',(-0.384119047314215,1.,1.71231062891398));
#26615=CARTESIAN_POINT('Ctrl Pts',(-0.383122945602004,-1.,1.7075470150345));
#26616=CARTESIAN_POINT('Ctrl Pts',(-0.383122945602004,1.,1.7075470150345));
#26617=CARTESIAN_POINT('',(-0.61342227326009,1.,2.11275013067528));
#26618=CARTESIAN_POINT('Ctrl Pts',(-0.61342227326009,1.,2.11275013067528));
#26619=CARTESIAN_POINT('Ctrl Pts',(-0.61246736556225,1.,2.11187554260142));
#26620=CARTESIAN_POINT('Ctrl Pts',(-0.610560911691113,1.,2.11012443807661));
#26621=CARTESIAN_POINT('Ctrl Pts',(-0.607711315456826,1.,2.10749199615859));
#26622=CARTESIAN_POINT('Ctrl Pts',(-0.603932030738212,1.,2.10397049887709));
#26623=CARTESIAN_POINT('Ctrl Pts',(-0.599241616422144,1.,2.09954930865331));
#26624=CARTESIAN_POINT('Ctrl Pts',(-0.594585006052824,1.,2.09510876220501));
#26625=CARTESIAN_POINT('Ctrl Pts',(-0.589962365403189,1.,2.09064881812053));
#26626=CARTESIAN_POINT('Ctrl Pts',(-0.585373918990895,1.,2.086169437277));
#26627=CARTESIAN_POINT('Ctrl Pts',(-0.580819952107257,1.,2.08167059018138));
#26628=CARTESIAN_POINT('Ctrl Pts',(-0.576300797416275,1.,2.07715226767361));
#26629=CARTESIAN_POINT('Ctrl Pts',(-0.571816823242411,1.,2.07261449292757));
#26630=CARTESIAN_POINT('Ctrl Pts',(-0.567368421181229,1.,2.06805732997383));
#26631=CARTESIAN_POINT('Ctrl Pts',(-0.562955993082574,1.,2.06348090160697));
#26632=CARTESIAN_POINT('Ctrl Pts',(-0.558579940185467,1.,2.05888537756571));
#26633=CARTESIAN_POINT('Ctrl Pts',(-0.55424065746411,1.,2.05427091604482));
#26634=CARTESIAN_POINT('Ctrl Pts',(-0.549938525150342,1.,2.04963761077974));
#26635=CARTESIAN_POINT('Ctrl Pts',(-0.545673903817348,1.,2.0449854471456));
#26636=CARTESIAN_POINT('Ctrl Pts',(-0.54144712061552,1.,2.0403142269048));
#26637=CARTESIAN_POINT('Ctrl Pts',(-0.537258489833134,1.,2.03562362953993));
#26638=CARTESIAN_POINT('Ctrl Pts',(-0.533108355132905,1.,2.03091336214401));
#26639=CARTESIAN_POINT('Ctrl Pts',(-0.528997127241911,1.,2.02618329083289));
#26640=CARTESIAN_POINT('Ctrl Pts',(-0.524925318333518,1.,2.02143356304712));
#26641=CARTESIAN_POINT('Ctrl Pts',(-0.520893590399428,1.,2.01666477917305));
#26642=CARTESIAN_POINT('Ctrl Pts',(-0.516902681728733,1.,2.01187773939257));
#26643=CARTESIAN_POINT('Ctrl Pts',(-0.512953306961814,1.,2.00707309946955));
#26644=CARTESIAN_POINT('Ctrl Pts',(-0.509046069886152,1.,2.00225107134733));
#26645=CARTESIAN_POINT('Ctrl Pts',(-0.505181361323011,1.,1.99741107463567));
#26646=CARTESIAN_POINT('Ctrl Pts',(-0.501359287727129,1.,1.9925514912615));
#26647=CARTESIAN_POINT('Ctrl Pts',(-0.497579909545564,1.,1.98767044752929));
#26648=CARTESIAN_POINT('Ctrl Pts',(-0.493843476541492,1.,1.9827665876182));
#26649=CARTESIAN_POINT('Ctrl Pts',(-0.490150627860955,1.,1.97783973019229));
#26650=CARTESIAN_POINT('Ctrl Pts',(-0.486502692907661,1.,1.97289186263272));
#26651=CARTESIAN_POINT('Ctrl Pts',(-0.482901662120687,1.,1.96792703422358));
#26652=CARTESIAN_POINT('Ctrl Pts',(-0.479349583074846,1.,1.96294933055938));
#26653=CARTESIAN_POINT('Ctrl Pts',(-0.475848034683172,1.,1.95796111148175));
#26654=CARTESIAN_POINT('Ctrl Pts',(-0.47239767226408,1.,1.95296148278136));
#26655=CARTESIAN_POINT('Ctrl Pts',(-0.468997482913158,1.,1.94794381136524));
#26656=CARTESIAN_POINT('Ctrl Pts',(-0.465645462026065,1.,1.94289794196205));
#26657=CARTESIAN_POINT('Ctrl Pts',(-0.462340031009087,1.,1.93781486640834));
#26658=CARTESIAN_POINT('Ctrl Pts',(-0.459081234547931,1.,1.93269066517936));
#26659=CARTESIAN_POINT('Ctrl Pts',(-0.455872005174335,1.,1.92753067150461));
#26660=CARTESIAN_POINT('Ctrl Pts',(-0.452719478359356,1.,1.9223538064847));
#26661=CARTESIAN_POINT('Ctrl Pts',(-0.449632260106572,1.,1.91718342555717));
#26662=CARTESIAN_POINT('Ctrl Pts',(-0.446617343485651,1.,1.91203699981095));
#26663=CARTESIAN_POINT('Ctrl Pts',(-0.44367755684917,1.,1.90691756144906));
#26664=CARTESIAN_POINT('Ctrl Pts',(-0.440807833704161,1.,1.90180124389137));
#26665=CARTESIAN_POINT('Ctrl Pts',(-0.437995003948443,1.,1.89663648956549));
#26666=CARTESIAN_POINT('Ctrl Pts',(-0.43522566096358,1.,1.89136993975585));
#26667=CARTESIAN_POINT('Ctrl Pts',(-0.432493038548833,1.,1.88596913666828));
#26668=CARTESIAN_POINT('Ctrl Pts',(-0.429803062482217,1.,1.88044229001778));
#26669=CARTESIAN_POINT('Ctrl Pts',(-0.427183828518743,1.,1.87486989291333));
#26670=CARTESIAN_POINT('Ctrl Pts',(-0.424678177290876,1.,1.8693780394412));
#26671=CARTESIAN_POINT('Ctrl Pts',(-0.422327307417885,1.,1.86408083333863));
#26672=CARTESIAN_POINT('Ctrl Pts',(-0.420157287975583,1.,1.8590328109667));
#26673=CARTESIAN_POINT('Ctrl Pts',(-0.418164129144045,1.,1.8541763285645));
#26674=CARTESIAN_POINT('Ctrl Pts',(-0.416300022039885,1.,1.84929312930314));
#26675=CARTESIAN_POINT('Ctrl Pts',(-0.414487438255542,1.,1.84405757074218));
#26676=CARTESIAN_POINT('Ctrl Pts',(-0.412633125322945,1.,1.8380895347617));
#26677=CARTESIAN_POINT('Ctrl Pts',(-0.410641256301276,1.,1.83100408895047));
#26678=CARTESIAN_POINT('Ctrl Pts',(-0.408428948106227,1.,1.82247022677562));
#26679=CARTESIAN_POINT('Ctrl Pts',(-0.405933518407175,1.,1.81223801812013));
#26680=CARTESIAN_POINT('Ctrl Pts',(-0.403107976163396,1.,1.80012077173238));
#26681=CARTESIAN_POINT('Ctrl Pts',(-0.399919403774155,1.,1.78598826343754));
#26682=CARTESIAN_POINT('Ctrl Pts',(-0.396346196110688,1.,1.76975560043442));
#26683=CARTESIAN_POINT('Ctrl Pts',(-0.392375812285395,1.,1.75137405310193));
#26684=CARTESIAN_POINT('Ctrl Pts',(-0.388877023502615,1.,1.73493170972829));
#26685=CARTESIAN_POINT('Ctrl Pts',(-0.386070790323281,1.,1.72162022244582));
#26686=CARTESIAN_POINT('Ctrl Pts',(-0.384119047314215,1.,1.71231062891398));
#26687=CARTESIAN_POINT('Ctrl Pts',(-0.383122945602004,1.,1.7075470150345));
#26688=CARTESIAN_POINT('',(-0.61342227326009,0.,2.11275013067528));
#26689=CARTESIAN_POINT('Origin',(-0.745574324794401,0.,2.0698113262342));
#26690=CARTESIAN_POINT('',(-0.745574324794401,1.,2.0698113262342));
#26691=CARTESIAN_POINT('',(-0.61342227326009,1.,2.11275013067528));
#26692=CARTESIAN_POINT('',(-0.745574324794401,0.,2.0698113262342));
#26693=CARTESIAN_POINT('Ctrl Pts',(-0.693717979106306,-1.,1.60662857109684));
#26694=CARTESIAN_POINT('Ctrl Pts',(-0.693717979106306,1.,1.60662857109684));
#26695=CARTESIAN_POINT('Ctrl Pts',(-0.695712097881194,-1.,1.61106790958151));
#26696=CARTESIAN_POINT('Ctrl Pts',(-0.695712097881194,1.,1.61106790958151));
#26697=CARTESIAN_POINT('Ctrl Pts',(-0.699605146405088,-1.,1.61974673472612));
#26698=CARTESIAN_POINT('Ctrl Pts',(-0.699605146405088,1.,1.61974673472612));
#26699=CARTESIAN_POINT('Ctrl Pts',(-0.705159151988319,-1.,1.63216541664676));
#26700=CARTESIAN_POINT('Ctrl Pts',(-0.705159151988319,1.,1.63216541664676));
#26701=CARTESIAN_POINT('Ctrl Pts',(-0.711993139355394,-1.,1.64752408832016));
#26702=CARTESIAN_POINT('Ctrl Pts',(-0.711993139355394,1.,1.64752408832016));
#26703=CARTESIAN_POINT('Ctrl Pts',(-0.719585433804282,-1.,1.6647288055568));
#26704=CARTESIAN_POINT('Ctrl Pts',(-0.719585433804282,1.,1.6647288055568));
#26705=CARTESIAN_POINT('Ctrl Pts',(-0.726235967997433,-1.,1.67996158455503));
#26706=CARTESIAN_POINT('Ctrl Pts',(-0.726235967997433,1.,1.67996158455503));
#26707=CARTESIAN_POINT('Ctrl Pts',(-0.731963238697195,-1.,1.69326921975743));
#26708=CARTESIAN_POINT('Ctrl Pts',(-0.731963238697195,1.,1.69326921975743));
#26709=CARTESIAN_POINT('Ctrl Pts',(-0.736799665724771,-1.,1.70473309006121));
#26710=CARTESIAN_POINT('Ctrl Pts',(-0.736799665724771,1.,1.70473309006121));
#26711=CARTESIAN_POINT('Ctrl Pts',(-0.740795162032088,-1.,1.71447789751927));
#26712=CARTESIAN_POINT('Ctrl Pts',(-0.740795162032088,1.,1.71447789751927));
#26713=CARTESIAN_POINT('Ctrl Pts',(-0.744021445433764,-1.,1.7226822991693));
#26714=CARTESIAN_POINT('Ctrl Pts',(-0.744021445433764,1.,1.7226822991693));
#26715=CARTESIAN_POINT('Ctrl Pts',(-0.746574710096436,-1.,1.72958533647399));
#26716=CARTESIAN_POINT('Ctrl Pts',(-0.746574710096436,1.,1.72958533647399));
#26717=CARTESIAN_POINT('Ctrl Pts',(-0.748582462954855,-1.,1.73550351679848));
#26718=CARTESIAN_POINT('Ctrl Pts',(-0.748582462954855,1.,1.73550351679848));
#26719=CARTESIAN_POINT('Ctrl Pts',(-0.75019343597954,-1.,1.74080458266705));
#26720=CARTESIAN_POINT('Ctrl Pts',(-0.75019343597954,1.,1.74080458266705));
#26721=CARTESIAN_POINT('Ctrl Pts',(-0.751555614163629,-1.,1.74585086852298));
#26722=CARTESIAN_POINT('Ctrl Pts',(-0.751555614163629,1.,1.74585086852298));
#26723=CARTESIAN_POINT('Ctrl Pts',(-0.752797683531377,-1.,1.75095139468809));
#26724=CARTESIAN_POINT('Ctrl Pts',(-0.752797683531377,1.,1.75095139468809));
#26725=CARTESIAN_POINT('Ctrl Pts',(-0.75400925402848,-1.,1.75631083600175));
#26726=CARTESIAN_POINT('Ctrl Pts',(-0.75400925402848,1.,1.75631083600175));
#26727=CARTESIAN_POINT('Ctrl Pts',(-0.755220979975262,-1.,1.7619781724032));
#26728=CARTESIAN_POINT('Ctrl Pts',(-0.755220979975262,1.,1.7619781724032));
#26729=CARTESIAN_POINT('Ctrl Pts',(-0.756421896028403,-1.,1.76789396003141));
#26730=CARTESIAN_POINT('Ctrl Pts',(-0.756421896028403,1.,1.76789396003141));
#26731=CARTESIAN_POINT('Ctrl Pts',(-0.757578264077238,-1.,1.77394167108342));
#26732=CARTESIAN_POINT('Ctrl Pts',(-0.757578264077238,1.,1.77394167108342));
#26733=CARTESIAN_POINT('Ctrl Pts',(-0.75865062667738,-1.,1.77999411220912));
#26734=CARTESIAN_POINT('Ctrl Pts',(-0.75865062667738,1.,1.77999411220912));
#26735=CARTESIAN_POINT('Ctrl Pts',(-0.759614401109868,-1.,1.78596964884526));
#26736=CARTESIAN_POINT('Ctrl Pts',(-0.759614401109868,1.,1.78596964884526));
#26737=CARTESIAN_POINT('Ctrl Pts',(-0.760469555880425,-1.,1.79185815610802));
#26738=CARTESIAN_POINT('Ctrl Pts',(-0.760469555880425,1.,1.79185815610802));
#26739=CARTESIAN_POINT('Ctrl Pts',(-0.761229695230359,-1.,1.79768986997735));
#26740=CARTESIAN_POINT('Ctrl Pts',(-0.761229695230359,1.,1.79768986997735));
#26741=CARTESIAN_POINT('Ctrl Pts',(-0.761915336443516,-1.,1.80351583877334));
#26742=CARTESIAN_POINT('Ctrl Pts',(-0.761915336443516,1.,1.80351583877334));
#26743=CARTESIAN_POINT('Ctrl Pts',(-0.762546129464036,-1.,1.80938551463989));
#26744=CARTESIAN_POINT('Ctrl Pts',(-0.762546129464036,1.,1.80938551463989));
#26745=CARTESIAN_POINT('Ctrl Pts',(-0.763132003836783,-1.,1.81532118405566));
#26746=CARTESIAN_POINT('Ctrl Pts',(-0.763132003836783,1.,1.81532118405566));
#26747=CARTESIAN_POINT('Ctrl Pts',(-0.763673465462854,-1.,1.82131873145297));
#26748=CARTESIAN_POINT('Ctrl Pts',(-0.763673465462854,1.,1.82131873145297));
#26749=CARTESIAN_POINT('Ctrl Pts',(-0.764165902606055,-1.,1.8273599120008));
#26750=CARTESIAN_POINT('Ctrl Pts',(-0.764165902606055,1.,1.8273599120008));
#26751=CARTESIAN_POINT('Ctrl Pts',(-0.764602549687845,-1.,1.8334207722714));
#26752=CARTESIAN_POINT('Ctrl Pts',(-0.764602549687845,1.,1.8334207722714));
#26753=CARTESIAN_POINT('Ctrl Pts',(-0.764978057881687,-1.,1.83948181064823));
#26754=CARTESIAN_POINT('Ctrl Pts',(-0.764978057881687,1.,1.83948181064823));
#26755=CARTESIAN_POINT('Ctrl Pts',(-0.765291664861971,-1.,1.8455369887591));
#26756=CARTESIAN_POINT('Ctrl Pts',(-0.765291664861971,1.,1.8455369887591));
#26757=CARTESIAN_POINT('Ctrl Pts',(-0.765545710619023,-1.,1.85158945130054));
#26758=CARTESIAN_POINT('Ctrl Pts',(-0.765545710619023,1.,1.85158945130054));
#26759=CARTESIAN_POINT('Ctrl Pts',(-0.765744212909305,-1.,1.85764741390391));
#26760=CARTESIAN_POINT('Ctrl Pts',(-0.765744212909305,1.,1.85764741390391));
#26761=CARTESIAN_POINT('Ctrl Pts',(-0.765891519092557,-1.,1.86372027063314));
#26762=CARTESIAN_POINT('Ctrl Pts',(-0.765891519092557,1.,1.86372027063314));
#26763=CARTESIAN_POINT('Ctrl Pts',(-0.765990708546111,-1.,1.86981398314345));
#26764=CARTESIAN_POINT('Ctrl Pts',(-0.765990708546111,1.,1.86981398314345));
#26765=CARTESIAN_POINT('Ctrl Pts',(-0.766042837036759,-1.,1.87592888967886));
#26766=CARTESIAN_POINT('Ctrl Pts',(-0.766042837036759,1.,1.87592888967886));
#26767=CARTESIAN_POINT('Ctrl Pts',(-0.766047794851869,-1.,1.88206215302561));
#26768=CARTESIAN_POINT('Ctrl Pts',(-0.766047794851869,1.,1.88206215302561));
#26769=CARTESIAN_POINT('Ctrl Pts',(-0.76600483706209,-1.,1.88820926433409));
#26770=CARTESIAN_POINT('Ctrl Pts',(-0.76600483706209,1.,1.88820926433409));
#26771=CARTESIAN_POINT('Ctrl Pts',(-0.765913193856979,-1.,1.89436577771389));
#26772=CARTESIAN_POINT('Ctrl Pts',(-0.765913193856979,1.,1.89436577771389));
#26773=CARTESIAN_POINT('Ctrl Pts',(-0.765772772593395,-1.,1.90052930393599));
#26774=CARTESIAN_POINT('Ctrl Pts',(-0.765772772593395,1.,1.90052930393599));
#26775=CARTESIAN_POINT('Ctrl Pts',(-0.765584196937936,-1.,1.90669961402362));
#26776=CARTESIAN_POINT('Ctrl Pts',(-0.765584196937936,1.,1.90669961402362));
#26777=CARTESIAN_POINT('Ctrl Pts',(-0.765348465884739,-1.,1.91287765805174));
#26778=CARTESIAN_POINT('Ctrl Pts',(-0.765348465884739,1.,1.91287765805174));
#26779=CARTESIAN_POINT('Ctrl Pts',(-0.765066729667095,-1.,1.91906491634197));
#26780=CARTESIAN_POINT('Ctrl Pts',(-0.765066729667095,1.,1.91906491634197));
#26781=CARTESIAN_POINT('Ctrl Pts',(-0.764740025488189,-1.,1.92526263537041));
#26782=CARTESIAN_POINT('Ctrl Pts',(-0.764740025488189,1.,1.92526263537041));
#26783=CARTESIAN_POINT('Ctrl Pts',(-0.764369010673889,-1.,1.93147105496367));
#26784=CARTESIAN_POINT('Ctrl Pts',(-0.764369010673889,1.,1.93147105496367));
#26785=CARTESIAN_POINT('Ctrl Pts',(-0.763954049121393,-1.,1.93768964875867));
#26786=CARTESIAN_POINT('Ctrl Pts',(-0.763954049121393,1.,1.93768964875867));
#26787=CARTESIAN_POINT('Ctrl Pts',(-0.76349533353858,-1.,1.94391746617626));
#26788=CARTESIAN_POINT('Ctrl Pts',(-0.76349533353858,1.,1.94391746617626));
#26789=CARTESIAN_POINT('Ctrl Pts',(-0.762992990878774,-1.,1.95015342590025));
#26790=CARTESIAN_POINT('Ctrl Pts',(-0.762992990878774,1.,1.95015342590025));
#26791=CARTESIAN_POINT('Ctrl Pts',(-0.762447203806263,-1.,1.95639665309893));
#26792=CARTESIAN_POINT('Ctrl Pts',(-0.762447203806263,1.,1.95639665309893));
#26793=CARTESIAN_POINT('Ctrl Pts',(-0.761858300014575,-1.,1.96264672744229));
#26794=CARTESIAN_POINT('Ctrl Pts',(-0.761858300014575,1.,1.96264672744229));
#26795=CARTESIAN_POINT('Ctrl Pts',(-0.761226690483986,-1.,1.96890351582545));
#26796=CARTESIAN_POINT('Ctrl Pts',(-0.761226690483986,1.,1.96890351582545));
#26797=CARTESIAN_POINT('Ctrl Pts',(-0.760552825409855,-1.,1.97516705321521));
#26798=CARTESIAN_POINT('Ctrl Pts',(-0.760552825409855,1.,1.97516705321521));
#26799=CARTESIAN_POINT('Ctrl Pts',(-0.759837147452135,-1.,1.98143741418156));
#26800=CARTESIAN_POINT('Ctrl Pts',(-0.759837147452135,1.,1.98143741418156));
#26801=CARTESIAN_POINT('Ctrl Pts',(-0.759080037802243,-1.,1.98771456680806));
#26802=CARTESIAN_POINT('Ctrl Pts',(-0.759080037802243,1.,1.98771456680806));
#26803=CARTESIAN_POINT('Ctrl Pts',(-0.758281796766377,-1.,1.9939983109871));
#26804=CARTESIAN_POINT('Ctrl Pts',(-0.758281796766377,1.,1.9939983109871));
#26805=CARTESIAN_POINT('Ctrl Pts',(-0.757442676862341,-1.,2.00028834739072));
#26806=CARTESIAN_POINT('Ctrl Pts',(-0.757442676862341,1.,2.00028834739072));
#26807=CARTESIAN_POINT('Ctrl Pts',(-0.756562904646496,-1.,2.00658431587682));
#26808=CARTESIAN_POINT('Ctrl Pts',(-0.756562904646496,1.,2.00658431587682));
#26809=CARTESIAN_POINT('Ctrl Pts',(-0.7556427049581,-1.,2.01288584328149));
#26810=CARTESIAN_POINT('Ctrl Pts',(-0.7556427049581,1.,2.01288584328149));
#26811=CARTESIAN_POINT('Ctrl Pts',(-0.75468233072352,-1.,2.01919259406003));
#26812=CARTESIAN_POINT('Ctrl Pts',(-0.75468233072352,1.,2.01919259406003));
#26813=CARTESIAN_POINT('Ctrl Pts',(-0.753682061113766,-1.,2.02550428623587));
#26814=CARTESIAN_POINT('Ctrl Pts',(-0.753682061113766,1.,2.02550428623587));
#26815=CARTESIAN_POINT('Ctrl Pts',(-0.752642180488104,-1.,2.03182068456467));
#26816=CARTESIAN_POINT('Ctrl Pts',(-0.752642180488104,1.,2.03182068456467));
#26817=CARTESIAN_POINT('Ctrl Pts',(-0.751562963361384,-1.,2.03814160092173));
#26818=CARTESIAN_POINT('Ctrl Pts',(-0.751562963361384,1.,2.03814160092173));
#26819=CARTESIAN_POINT('Ctrl Pts',(-0.750444657874758,-1.,2.04446689147754));
#26820=CARTESIAN_POINT('Ctrl Pts',(-0.750444657874758,1.,2.04446689147754));
#26821=CARTESIAN_POINT('Ctrl Pts',(-0.749287468663053,-1.,2.05079645591606));
#26822=CARTESIAN_POINT('Ctrl Pts',(-0.749287468663053,1.,2.05079645591606));
#26823=CARTESIAN_POINT('Ctrl Pts',(-0.748091554181101,-1.,2.05713023030263));
#26824=CARTESIAN_POINT('Ctrl Pts',(-0.748091554181101,1.,2.05713023030263));
#26825=CARTESIAN_POINT('Ctrl Pts',(-0.747103932785504,-1.,2.06220058927162));
#26826=CARTESIAN_POINT('Ctrl Pts',(-0.747103932785504,1.,2.06220058927162));
#26827=CARTESIAN_POINT('Ctrl Pts',(-0.746345871542696,-1.,2.06600523016401));
#26828=CARTESIAN_POINT('Ctrl Pts',(-0.746345871542696,1.,2.06600523016401));
#26829=CARTESIAN_POINT('Ctrl Pts',(-0.74583279137781,-1.,2.06854248895575));
#26830=CARTESIAN_POINT('Ctrl Pts',(-0.74583279137781,1.,2.06854248895575));
#26831=CARTESIAN_POINT('Ctrl Pts',(-0.745574324794401,-1.,2.0698113262342));
#26832=CARTESIAN_POINT('Ctrl Pts',(-0.745574324794401,1.,2.0698113262342));
#26833=CARTESIAN_POINT('',(-0.693717979106306,1.,1.60662857109684));
#26834=CARTESIAN_POINT('Ctrl Pts',(-0.693717979106306,1.,1.60662857109684));
#26835=CARTESIAN_POINT('Ctrl Pts',(-0.695712097881194,1.,1.61106790958151));
#26836=CARTESIAN_POINT('Ctrl Pts',(-0.699605146405088,1.,1.61974673472612));
#26837=CARTESIAN_POINT('Ctrl Pts',(-0.705159151988319,1.,1.63216541664676));
#26838=CARTESIAN_POINT('Ctrl Pts',(-0.711993139355394,1.,1.64752408832016));
#26839=CARTESIAN_POINT('Ctrl Pts',(-0.719585433804282,1.,1.6647288055568));
#26840=CARTESIAN_POINT('Ctrl Pts',(-0.726235967997433,1.,1.67996158455503));
#26841=CARTESIAN_POINT('Ctrl Pts',(-0.731963238697195,1.,1.69326921975743));
#26842=CARTESIAN_POINT('Ctrl Pts',(-0.736799665724771,1.,1.70473309006121));
#26843=CARTESIAN_POINT('Ctrl Pts',(-0.740795162032088,1.,1.71447789751927));
#26844=CARTESIAN_POINT('Ctrl Pts',(-0.744021445433764,1.,1.7226822991693));
#26845=CARTESIAN_POINT('Ctrl Pts',(-0.746574710096436,1.,1.72958533647399));
#26846=CARTESIAN_POINT('Ctrl Pts',(-0.748582462954855,1.,1.73550351679848));
#26847=CARTESIAN_POINT('Ctrl Pts',(-0.75019343597954,1.,1.74080458266705));
#26848=CARTESIAN_POINT('Ctrl Pts',(-0.751555614163629,1.,1.74585086852298));
#26849=CARTESIAN_POINT('Ctrl Pts',(-0.752797683531377,1.,1.75095139468809));
#26850=CARTESIAN_POINT('Ctrl Pts',(-0.75400925402848,1.,1.75631083600175));
#26851=CARTESIAN_POINT('Ctrl Pts',(-0.755220979975262,1.,1.7619781724032));
#26852=CARTESIAN_POINT('Ctrl Pts',(-0.756421896028403,1.,1.76789396003141));
#26853=CARTESIAN_POINT('Ctrl Pts',(-0.757578264077238,1.,1.77394167108342));
#26854=CARTESIAN_POINT('Ctrl Pts',(-0.75865062667738,1.,1.77999411220912));
#26855=CARTESIAN_POINT('Ctrl Pts',(-0.759614401109868,1.,1.78596964884526));
#26856=CARTESIAN_POINT('Ctrl Pts',(-0.760469555880425,1.,1.79185815610802));
#26857=CARTESIAN_POINT('Ctrl Pts',(-0.761229695230359,1.,1.79768986997735));
#26858=CARTESIAN_POINT('Ctrl Pts',(-0.761915336443516,1.,1.80351583877334));
#26859=CARTESIAN_POINT('Ctrl Pts',(-0.762546129464036,1.,1.80938551463989));
#26860=CARTESIAN_POINT('Ctrl Pts',(-0.763132003836783,1.,1.81532118405566));
#26861=CARTESIAN_POINT('Ctrl Pts',(-0.763673465462854,1.,1.82131873145297));
#26862=CARTESIAN_POINT('Ctrl Pts',(-0.764165902606055,1.,1.8273599120008));
#26863=CARTESIAN_POINT('Ctrl Pts',(-0.764602549687845,1.,1.8334207722714));
#26864=CARTESIAN_POINT('Ctrl Pts',(-0.764978057881687,1.,1.83948181064823));
#26865=CARTESIAN_POINT('Ctrl Pts',(-0.765291664861971,1.,1.8455369887591));
#26866=CARTESIAN_POINT('Ctrl Pts',(-0.765545710619023,1.,1.85158945130054));
#26867=CARTESIAN_POINT('Ctrl Pts',(-0.765744212909305,1.,1.85764741390391));
#26868=CARTESIAN_POINT('Ctrl Pts',(-0.765891519092557,1.,1.86372027063314));
#26869=CARTESIAN_POINT('Ctrl Pts',(-0.765990708546111,1.,1.86981398314345));
#26870=CARTESIAN_POINT('Ctrl Pts',(-0.766042837036759,1.,1.87592888967886));
#26871=CARTESIAN_POINT('Ctrl Pts',(-0.766047794851869,1.,1.88206215302561));
#26872=CARTESIAN_POINT('Ctrl Pts',(-0.76600483706209,1.,1.88820926433409));
#26873=CARTESIAN_POINT('Ctrl Pts',(-0.765913193856979,1.,1.89436577771389));
#26874=CARTESIAN_POINT('Ctrl Pts',(-0.765772772593395,1.,1.90052930393599));
#26875=CARTESIAN_POINT('Ctrl Pts',(-0.765584196937936,1.,1.90669961402362));
#26876=CARTESIAN_POINT('Ctrl Pts',(-0.765348465884739,1.,1.91287765805174));
#26877=CARTESIAN_POINT('Ctrl Pts',(-0.765066729667095,1.,1.91906491634197));
#26878=CARTESIAN_POINT('Ctrl Pts',(-0.764740025488189,1.,1.92526263537041));
#26879=CARTESIAN_POINT('Ctrl Pts',(-0.764369010673889,1.,1.93147105496367));
#26880=CARTESIAN_POINT('Ctrl Pts',(-0.763954049121393,1.,1.93768964875867));
#26881=CARTESIAN_POINT('Ctrl Pts',(-0.76349533353858,1.,1.94391746617626));
#26882=CARTESIAN_POINT('Ctrl Pts',(-0.762992990878774,1.,1.95015342590025));
#26883=CARTESIAN_POINT('Ctrl Pts',(-0.762447203806263,1.,1.95639665309893));
#26884=CARTESIAN_POINT('Ctrl Pts',(-0.761858300014575,1.,1.96264672744229));
#26885=CARTESIAN_POINT('Ctrl Pts',(-0.761226690483986,1.,1.96890351582545));
#26886=CARTESIAN_POINT('Ctrl Pts',(-0.760552825409855,1.,1.97516705321521));
#26887=CARTESIAN_POINT('Ctrl Pts',(-0.759837147452135,1.,1.98143741418156));
#26888=CARTESIAN_POINT('Ctrl Pts',(-0.759080037802243,1.,1.98771456680806));
#26889=CARTESIAN_POINT('Ctrl Pts',(-0.758281796766377,1.,1.9939983109871));
#26890=CARTESIAN_POINT('Ctrl Pts',(-0.757442676862341,1.,2.00028834739072));
#26891=CARTESIAN_POINT('Ctrl Pts',(-0.756562904646496,1.,2.00658431587682));
#26892=CARTESIAN_POINT('Ctrl Pts',(-0.7556427049581,1.,2.01288584328149));
#26893=CARTESIAN_POINT('Ctrl Pts',(-0.75468233072352,1.,2.01919259406003));
#26894=CARTESIAN_POINT('Ctrl Pts',(-0.753682061113766,1.,2.02550428623587));
#26895=CARTESIAN_POINT('Ctrl Pts',(-0.752642180488104,1.,2.03182068456467));
#26896=CARTESIAN_POINT('Ctrl Pts',(-0.751562963361384,1.,2.03814160092173));
#26897=CARTESIAN_POINT('Ctrl Pts',(-0.750444657874758,1.,2.04446689147754));
#26898=CARTESIAN_POINT('Ctrl Pts',(-0.749287468663053,1.,2.05079645591606));
#26899=CARTESIAN_POINT('Ctrl Pts',(-0.748091554181101,1.,2.05713023030263));
#26900=CARTESIAN_POINT('Ctrl Pts',(-0.747103932785504,1.,2.06220058927162));
#26901=CARTESIAN_POINT('Ctrl Pts',(-0.746345871542696,1.,2.06600523016401));
#26902=CARTESIAN_POINT('Ctrl Pts',(-0.74583279137781,1.,2.06854248895575));
#26903=CARTESIAN_POINT('Ctrl Pts',(-0.745574324794401,1.,2.0698113262342));
#26904=CARTESIAN_POINT('',(-0.693717979106306,0.,1.60662857109684));
#26905=CARTESIAN_POINT('Origin',(0.,0.,0.));
#26906=CARTESIAN_POINT('',(-0.892032620296855,1.,1.5055822144029));
#26907=CARTESIAN_POINT('Origin',(0.,1.,0.));
#26908=CARTESIAN_POINT('',(-0.892032620296855,0.,1.5055822144029));
#26909=CARTESIAN_POINT('Ctrl Pts',(-1.23627494547115,-1.,1.81978687191668));
#26910=CARTESIAN_POINT('Ctrl Pts',(-1.23627494547115,1.,1.81978687191668));
#26911=CARTESIAN_POINT('Ctrl Pts',(-1.23509651170476,-1.,1.81925017193666));
#26912=CARTESIAN_POINT('Ctrl Pts',(-1.23509651170476,1.,1.81925017193666));
#26913=CARTESIAN_POINT('Ctrl Pts',(-1.2327422452705,-1.,1.81817389921279));
#26914=CARTESIAN_POINT('Ctrl Pts',(-1.2327422452705,1.,1.81817389921279));
#26915=CARTESIAN_POINT('Ctrl Pts',(-1.2292186489137,-1.,1.8165508718364));
#26916=CARTESIAN_POINT('Ctrl Pts',(-1.2292186489137,1.,1.8165508718364));
#26917=CARTESIAN_POINT('Ctrl Pts',(-1.2245361330495,-1.,1.81436959210434));
#26918=CARTESIAN_POINT('Ctrl Pts',(-1.2245361330495,1.,1.81436959210434));
#26919=CARTESIAN_POINT('Ctrl Pts',(-1.21870906103557,-1.,1.81161420806656));
#26920=CARTESIAN_POINT('Ctrl Pts',(-1.21870906103557,1.,1.81161420806656));
#26921=CARTESIAN_POINT('Ctrl Pts',(-1.21290815708314,-1.,1.80882996917129));
#26922=CARTESIAN_POINT('Ctrl Pts',(-1.21290815708314,1.,1.80882996917129));
#26923=CARTESIAN_POINT('Ctrl Pts',(-1.20713356605475,-1.,1.80601678480707));
#26924=CARTESIAN_POINT('Ctrl Pts',(-1.20713356605475,1.,1.80601678480707));
#26925=CARTESIAN_POINT('Ctrl Pts',(-1.20138548938974,-1.,1.80317454838603));
#26926=CARTESIAN_POINT('Ctrl Pts',(-1.20138548938974,1.,1.80317454838603));
#26927=CARTESIAN_POINT('Ctrl Pts',(-1.19566418930242,-1.,1.80030314369879));
#26928=CARTESIAN_POINT('Ctrl Pts',(-1.19566418930242,1.,1.80030314369879));
#26929=CARTESIAN_POINT('Ctrl Pts',(-1.18996997934445,-1.,1.79740245923478));
#26930=CARTESIAN_POINT('Ctrl Pts',(-1.18996997934445,1.,1.79740245923478));
#26931=CARTESIAN_POINT('Ctrl Pts',(-1.18430321697432,-1.,1.79447240321515));
#26932=CARTESIAN_POINT('Ctrl Pts',(-1.18430321697432,1.,1.79447240321515));
#26933=CARTESIAN_POINT('Ctrl Pts',(-1.17866429440809,-1.,1.79151291552689));
#26934=CARTESIAN_POINT('Ctrl Pts',(-1.17866429440809,1.,1.79151291552689));
#26935=CARTESIAN_POINT('Ctrl Pts',(-1.17305363177328,-1.,1.78852398877616));
#26936=CARTESIAN_POINT('Ctrl Pts',(-1.17305363177328,1.,1.78852398877616));
#26937=CARTESIAN_POINT('Ctrl Pts',(-1.16747166312303,-1.,1.78550566040443));
#26938=CARTESIAN_POINT('Ctrl Pts',(-1.16747166312303,1.,1.78550566040443));
#26939=CARTESIAN_POINT('Ctrl Pts',(-1.16191881298499,-1.,1.78245795881009));
#26940=CARTESIAN_POINT('Ctrl Pts',(-1.16191881298499,1.,1.78245795881009));
#26941=CARTESIAN_POINT('Ctrl Pts',(-1.15639547194698,-1.,1.77938085564275));
#26942=CARTESIAN_POINT('Ctrl Pts',(-1.15639547194698,1.,1.77938085564275));
#26943=CARTESIAN_POINT('Ctrl Pts',(-1.15090197841515,-1.,1.7762742255701));
#26944=CARTESIAN_POINT('Ctrl Pts',(-1.15090197841515,1.,1.7762742255701));
#26945=CARTESIAN_POINT('Ctrl Pts',(-1.1454385822692,-1.,1.77313777896194));
#26946=CARTESIAN_POINT('Ctrl Pts',(-1.1454385822692,1.,1.77313777896194));
#26947=CARTESIAN_POINT('Ctrl Pts',(-1.14000548336975,-1.,1.76997111386769));
#26948=CARTESIAN_POINT('Ctrl Pts',(-1.14000548336975,1.,1.76997111386769));
#26949=CARTESIAN_POINT('Ctrl Pts',(-1.1346029180462,-1.,1.76677384551862));
#26950=CARTESIAN_POINT('Ctrl Pts',(-1.1346029180462,1.,1.76677384551862));
#26951=CARTESIAN_POINT('Ctrl Pts',(-1.12923123555075,-1.,1.7635457196617));
#26952=CARTESIAN_POINT('Ctrl Pts',(-1.12923123555075,1.,1.7635457196617));
#26953=CARTESIAN_POINT('Ctrl Pts',(-1.12389096855086,-1.,1.76028671825096));
#26954=CARTESIAN_POINT('Ctrl Pts',(-1.12389096855086,1.,1.76028671825096));
#26955=CARTESIAN_POINT('Ctrl Pts',(-1.11858293216763,-1.,1.75699720772105));
#26956=CARTESIAN_POINT('Ctrl Pts',(-1.11858293216763,1.,1.75699720772105));
#26957=CARTESIAN_POINT('Ctrl Pts',(-1.11330807582551,-1.,1.7536777209463));
#26958=CARTESIAN_POINT('Ctrl Pts',(-1.11330807582551,1.,1.7536777209463));
#26959=CARTESIAN_POINT('Ctrl Pts',(-1.10806728183007,-1.,1.7503286607592));
#26960=CARTESIAN_POINT('Ctrl Pts',(-1.10806728183007,1.,1.7503286607592));
#26961=CARTESIAN_POINT('Ctrl Pts',(-1.10286118991143,-1.,1.74695004214923));
#26962=CARTESIAN_POINT('Ctrl Pts',(-1.10286118991143,1.,1.74695004214923));
#26963=CARTESIAN_POINT('Ctrl Pts',(-1.09768999241225,-1.,1.74354119236208));
#26964=CARTESIAN_POINT('Ctrl Pts',(-1.09768999241225,1.,1.74354119236208));
#26965=CARTESIAN_POINT('Ctrl Pts',(-1.09255329056493,-1.,1.74010053962247));
#26966=CARTESIAN_POINT('Ctrl Pts',(-1.09255329056493,1.,1.74010053962247));
#26967=CARTESIAN_POINT('Ctrl Pts',(-1.08745056285427,-1.,1.73662628326091));
#26968=CARTESIAN_POINT('Ctrl Pts',(-1.08745056285427,1.,1.73662628326091));
#26969=CARTESIAN_POINT('Ctrl Pts',(-1.08238162784749,-1.,1.73311705663407));
#26970=CARTESIAN_POINT('Ctrl Pts',(-1.08238162784749,1.,1.73311705663407));
#26971=CARTESIAN_POINT('Ctrl Pts',(-1.0773470373727,-1.,1.72957248977424));
#26972=CARTESIAN_POINT('Ctrl Pts',(-1.0773470373727,1.,1.72957248977424));
#26973=CARTESIAN_POINT('Ctrl Pts',(-1.07234866990252,-1.,1.72599406198488));
#26974=CARTESIAN_POINT('Ctrl Pts',(-1.07234866990252,1.,1.72599406198488));
#26975=CARTESIAN_POINT('Ctrl Pts',(-1.06738966975462,-1.,1.72238500928453));
#26976=CARTESIAN_POINT('Ctrl Pts',(-1.06738966975462,1.,1.72238500928453));
#26977=CARTESIAN_POINT('Ctrl Pts',(-1.06247324680647,-1.,1.71874858456904));
#26978=CARTESIAN_POINT('Ctrl Pts',(-1.06247324680647,1.,1.71874858456904));
#26979=CARTESIAN_POINT('Ctrl Pts',(-1.05760163192479,-1.,1.7150865442702));
#26980=CARTESIAN_POINT('Ctrl Pts',(-1.05760163192479,1.,1.7150865442702));
#26981=CARTESIAN_POINT('Ctrl Pts',(-1.05277517202855,-1.,1.71139783543989));
#26982=CARTESIAN_POINT('Ctrl Pts',(-1.05277517202855,1.,1.71139783543989));
#26983=CARTESIAN_POINT('Ctrl Pts',(-1.04799085404995,-1.,1.70767646263649));
#26984=CARTESIAN_POINT('Ctrl Pts',(-1.04799085404995,1.,1.70767646263649));
#26985=CARTESIAN_POINT('Ctrl Pts',(-1.04324363334554,-1.,1.70391338707982));
#26986=CARTESIAN_POINT('Ctrl Pts',(-1.04324363334554,1.,1.70391338707982));
#26987=CARTESIAN_POINT('Ctrl Pts',(-1.03852922490789,-1.,1.70010052930962));
#26988=CARTESIAN_POINT('Ctrl Pts',(-1.03852922490789,1.,1.70010052930962));
#26989=CARTESIAN_POINT('Ctrl Pts',(-1.03384646003588,-1.,1.69623414782771));
#26990=CARTESIAN_POINT('Ctrl Pts',(-1.03384646003588,1.,1.69623414782771));
#26991=CARTESIAN_POINT('Ctrl Pts',(-1.02919977579147,-1.,1.69231840863458));
#26992=CARTESIAN_POINT('Ctrl Pts',(-1.02919977579147,1.,1.69231840863458));
#26993=CARTESIAN_POINT('Ctrl Pts',(-1.02460180535255,-1.,1.68836910178447));
#26994=CARTESIAN_POINT('Ctrl Pts',(-1.02460180535255,1.,1.68836910178447));
#26995=CARTESIAN_POINT('Ctrl Pts',(-1.02006795074201,-1.,1.68440578021706));
#26996=CARTESIAN_POINT('Ctrl Pts',(-1.02006795074201,1.,1.68440578021706));
#26997=CARTESIAN_POINT('Ctrl Pts',(-1.01561026162773,-1.,1.68044289894798));
#26998=CARTESIAN_POINT('Ctrl Pts',(-1.01561026162773,1.,1.68044289894798));
#26999=CARTESIAN_POINT('Ctrl Pts',(-1.01123236493511,-1.,1.67648246776464));
#27000=CARTESIAN_POINT('Ctrl Pts',(-1.01123236493511,1.,1.67648246776464));
#27001=CARTESIAN_POINT('Ctrl Pts',(-1.00692206696414,-1.,1.67250335383293));
#27002=CARTESIAN_POINT('Ctrl Pts',(-1.00692206696414,1.,1.67250335383293));
#27003=CARTESIAN_POINT('Ctrl Pts',(-1.00265091003727,-1.,1.66846059277303));
#27004=CARTESIAN_POINT('Ctrl Pts',(-1.00265091003727,1.,1.66846059277303));
#27005=CARTESIAN_POINT('Ctrl Pts',(-0.998389654952758,-1.,1.66430758030376));
#27006=CARTESIAN_POINT('Ctrl Pts',(-0.998389654952758,1.,1.66430758030376));
#27007=CARTESIAN_POINT('Ctrl Pts',(-0.994121836661306,-1.,1.66001553809947));
#27008=CARTESIAN_POINT('Ctrl Pts',(-0.994121836661306,1.,1.66001553809947));
#27009=CARTESIAN_POINT('Ctrl Pts',(-0.989855627854165,-1.,1.65559044289699));
#27010=CARTESIAN_POINT('Ctrl Pts',(-0.989855627854165,1.,1.65559044289699));
#27011=CARTESIAN_POINT('Ctrl Pts',(-0.985642622920821,-1.,1.65110016612638));
#27012=CARTESIAN_POINT('Ctrl Pts',(-0.985642622920821,1.,1.65110016612638));
#27013=CARTESIAN_POINT('Ctrl Pts',(-0.981562530939489,-1.,1.64665139190656));
#27014=CARTESIAN_POINT('Ctrl Pts',(-0.981562530939489,1.,1.64665139190656));
#27015=CARTESIAN_POINT('Ctrl Pts',(-0.977689794119416,-1.,1.64233990826687));
#27016=CARTESIAN_POINT('Ctrl Pts',(-0.977689794119416,1.,1.64233990826687));
#27017=CARTESIAN_POINT('Ctrl Pts',(-0.974066058287418,-1.,1.63820952658144));
#27018=CARTESIAN_POINT('Ctrl Pts',(-0.974066058287418,1.,1.63820952658144));
#27019=CARTESIAN_POINT('Ctrl Pts',(-0.970669715997509,-1.,1.63420665729798));
#27020=CARTESIAN_POINT('Ctrl Pts',(-0.970669715997509,1.,1.63420665729798));
#27021=CARTESIAN_POINT('Ctrl Pts',(-0.967387853230345,-1.,1.63013849959461));
#27022=CARTESIAN_POINT('Ctrl Pts',(-0.967387853230345,1.,1.63013849959461));
#27023=CARTESIAN_POINT('Ctrl Pts',(-0.964046107040536,-1.,1.62571930670187));
#27024=CARTESIAN_POINT('Ctrl Pts',(-0.964046107040536,1.,1.62571930670187));
#27025=CARTESIAN_POINT('Ctrl Pts',(-0.960438326101729,-1.,1.62061638140221));
#27026=CARTESIAN_POINT('Ctrl Pts',(-0.960438326101729,1.,1.62061638140221));
#27027=CARTESIAN_POINT('Ctrl Pts',(-0.956354422920671,-1.,1.61449324337085));
#27028=CARTESIAN_POINT('Ctrl Pts',(-0.956354422920671,1.,1.61449324337085));
#27029=CARTESIAN_POINT('Ctrl Pts',(-0.951613284356035,-1.,1.60706069896936));
#27030=CARTESIAN_POINT('Ctrl Pts',(-0.951613284356035,1.,1.60706069896936));
#27031=CARTESIAN_POINT('Ctrl Pts',(-0.946078063315257,-1.,1.59810042043673));
#27032=CARTESIAN_POINT('Ctrl Pts',(-0.946078063315257,1.,1.59810042043673));
#27033=CARTESIAN_POINT('Ctrl Pts',(-0.939646377893399,-1.,1.58744937487176));
#27034=CARTESIAN_POINT('Ctrl Pts',(-0.939646377893399,1.,1.58744937487176));
#27035=CARTESIAN_POINT('Ctrl Pts',(-0.932246680108685,-1.,1.57499388382243));
#27036=CARTESIAN_POINT('Ctrl Pts',(-0.932246680108685,1.,1.57499388382243));
#27037=CARTESIAN_POINT('Ctrl Pts',(-0.923832188944341,-1.,1.56065988578893));
#27038=CARTESIAN_POINT('Ctrl Pts',(-0.923832188944341,1.,1.56065988578893));
#27039=CARTESIAN_POINT('Ctrl Pts',(-0.914375919026456,-1.,1.54440491149498));
#27040=CARTESIAN_POINT('Ctrl Pts',(-0.914375919026456,1.,1.54440491149498));
#27041=CARTESIAN_POINT('Ctrl Pts',(-0.905967409625651,-1.,1.52984849887993));
#27042=CARTESIAN_POINT('Ctrl Pts',(-0.905967409625651,1.,1.52984849887993));
#27043=CARTESIAN_POINT('Ctrl Pts',(-0.899185047483511,-1.,1.51805569590094));
#27044=CARTESIAN_POINT('Ctrl Pts',(-0.899185047483511,1.,1.51805569590094));
#27045=CARTESIAN_POINT('Ctrl Pts',(-0.894452006964543,-1.,1.50980486806688));
#27046=CARTESIAN_POINT('Ctrl Pts',(-0.894452006964543,1.,1.50980486806688));
#27047=CARTESIAN_POINT('Ctrl Pts',(-0.892032620296855,-1.,1.5055822144029));
#27048=CARTESIAN_POINT('Ctrl Pts',(-0.892032620296855,1.,1.5055822144029));
#27049=CARTESIAN_POINT('',(-1.23627494547115,1.,1.81978687191668));
#27050=CARTESIAN_POINT('Ctrl Pts',(-1.23627494547115,1.,1.81978687191668));
#27051=CARTESIAN_POINT('Ctrl Pts',(-1.23509651170476,1.,1.81925017193666));
#27052=CARTESIAN_POINT('Ctrl Pts',(-1.2327422452705,1.,1.81817389921279));
#27053=CARTESIAN_POINT('Ctrl Pts',(-1.2292186489137,1.,1.8165508718364));
#27054=CARTESIAN_POINT('Ctrl Pts',(-1.2245361330495,1.,1.81436959210434));
#27055=CARTESIAN_POINT('Ctrl Pts',(-1.21870906103557,1.,1.81161420806656));
#27056=CARTESIAN_POINT('Ctrl Pts',(-1.21290815708314,1.,1.80882996917129));
#27057=CARTESIAN_POINT('Ctrl Pts',(-1.20713356605475,1.,1.80601678480707));
#27058=CARTESIAN_POINT('Ctrl Pts',(-1.20138548938974,1.,1.80317454838603));
#27059=CARTESIAN_POINT('Ctrl Pts',(-1.19566418930242,1.,1.80030314369879));
#27060=CARTESIAN_POINT('Ctrl Pts',(-1.18996997934445,1.,1.79740245923478));
#27061=CARTESIAN_POINT('Ctrl Pts',(-1.18430321697432,1.,1.79447240321515));
#27062=CARTESIAN_POINT('Ctrl Pts',(-1.17866429440809,1.,1.79151291552689));
#27063=CARTESIAN_POINT('Ctrl Pts',(-1.17305363177328,1.,1.78852398877616));
#27064=CARTESIAN_POINT('Ctrl Pts',(-1.16747166312303,1.,1.78550566040443));
#27065=CARTESIAN_POINT('Ctrl Pts',(-1.16191881298499,1.,1.78245795881009));
#27066=CARTESIAN_POINT('Ctrl Pts',(-1.15639547194698,1.,1.77938085564275));
#27067=CARTESIAN_POINT('Ctrl Pts',(-1.15090197841515,1.,1.7762742255701));
#27068=CARTESIAN_POINT('Ctrl Pts',(-1.1454385822692,1.,1.77313777896194));
#27069=CARTESIAN_POINT('Ctrl Pts',(-1.14000548336975,1.,1.76997111386769));
#27070=CARTESIAN_POINT('Ctrl Pts',(-1.1346029180462,1.,1.76677384551862));
#27071=CARTESIAN_POINT('Ctrl Pts',(-1.12923123555075,1.,1.7635457196617));
#27072=CARTESIAN_POINT('Ctrl Pts',(-1.12389096855086,1.,1.76028671825096));
#27073=CARTESIAN_POINT('Ctrl Pts',(-1.11858293216763,1.,1.75699720772105));
#27074=CARTESIAN_POINT('Ctrl Pts',(-1.11330807582551,1.,1.7536777209463));
#27075=CARTESIAN_POINT('Ctrl Pts',(-1.10806728183007,1.,1.7503286607592));
#27076=CARTESIAN_POINT('Ctrl Pts',(-1.10286118991143,1.,1.74695004214923));
#27077=CARTESIAN_POINT('Ctrl Pts',(-1.09768999241225,1.,1.74354119236208));
#27078=CARTESIAN_POINT('Ctrl Pts',(-1.09255329056493,1.,1.74010053962247));
#27079=CARTESIAN_POINT('Ctrl Pts',(-1.08745056285427,1.,1.73662628326091));
#27080=CARTESIAN_POINT('Ctrl Pts',(-1.08238162784749,1.,1.73311705663407));
#27081=CARTESIAN_POINT('Ctrl Pts',(-1.0773470373727,1.,1.72957248977424));
#27082=CARTESIAN_POINT('Ctrl Pts',(-1.07234866990252,1.,1.72599406198488));
#27083=CARTESIAN_POINT('Ctrl Pts',(-1.06738966975462,1.,1.72238500928453));
#27084=CARTESIAN_POINT('Ctrl Pts',(-1.06247324680647,1.,1.71874858456904));
#27085=CARTESIAN_POINT('Ctrl Pts',(-1.05760163192479,1.,1.7150865442702));
#27086=CARTESIAN_POINT('Ctrl Pts',(-1.05277517202855,1.,1.71139783543989));
#27087=CARTESIAN_POINT('Ctrl Pts',(-1.04799085404995,1.,1.70767646263649));
#27088=CARTESIAN_POINT('Ctrl Pts',(-1.04324363334554,1.,1.70391338707982));
#27089=CARTESIAN_POINT('Ctrl Pts',(-1.03852922490789,1.,1.70010052930962));
#27090=CARTESIAN_POINT('Ctrl Pts',(-1.03384646003588,1.,1.69623414782771));
#27091=CARTESIAN_POINT('Ctrl Pts',(-1.02919977579147,1.,1.69231840863458));
#27092=CARTESIAN_POINT('Ctrl Pts',(-1.02460180535255,1.,1.68836910178447));
#27093=CARTESIAN_POINT('Ctrl Pts',(-1.02006795074201,1.,1.68440578021706));
#27094=CARTESIAN_POINT('Ctrl Pts',(-1.01561026162773,1.,1.68044289894798));
#27095=CARTESIAN_POINT('Ctrl Pts',(-1.01123236493511,1.,1.67648246776464));
#27096=CARTESIAN_POINT('Ctrl Pts',(-1.00692206696414,1.,1.67250335383293));
#27097=CARTESIAN_POINT('Ctrl Pts',(-1.00265091003727,1.,1.66846059277303));
#27098=CARTESIAN_POINT('Ctrl Pts',(-0.998389654952758,1.,1.66430758030376));
#27099=CARTESIAN_POINT('Ctrl Pts',(-0.994121836661306,1.,1.66001553809947));
#27100=CARTESIAN_POINT('Ctrl Pts',(-0.989855627854165,1.,1.65559044289699));
#27101=CARTESIAN_POINT('Ctrl Pts',(-0.985642622920821,1.,1.65110016612638));
#27102=CARTESIAN_POINT('Ctrl Pts',(-0.981562530939489,1.,1.64665139190656));
#27103=CARTESIAN_POINT('Ctrl Pts',(-0.977689794119416,1.,1.64233990826687));
#27104=CARTESIAN_POINT('Ctrl Pts',(-0.974066058287418,1.,1.63820952658144));
#27105=CARTESIAN_POINT('Ctrl Pts',(-0.970669715997509,1.,1.63420665729798));
#27106=CARTESIAN_POINT('Ctrl Pts',(-0.967387853230345,1.,1.63013849959461));
#27107=CARTESIAN_POINT('Ctrl Pts',(-0.964046107040536,1.,1.62571930670187));
#27108=CARTESIAN_POINT('Ctrl Pts',(-0.960438326101729,1.,1.62061638140221));
#27109=CARTESIAN_POINT('Ctrl Pts',(-0.956354422920671,1.,1.61449324337085));
#27110=CARTESIAN_POINT('Ctrl Pts',(-0.951613284356035,1.,1.60706069896936));
#27111=CARTESIAN_POINT('Ctrl Pts',(-0.946078063315257,1.,1.59810042043673));
#27112=CARTESIAN_POINT('Ctrl Pts',(-0.939646377893399,1.,1.58744937487176));
#27113=CARTESIAN_POINT('Ctrl Pts',(-0.932246680108685,1.,1.57499388382243));
#27114=CARTESIAN_POINT('Ctrl Pts',(-0.923832188944341,1.,1.56065988578893));
#27115=CARTESIAN_POINT('Ctrl Pts',(-0.914375919026456,1.,1.54440491149498));
#27116=CARTESIAN_POINT('Ctrl Pts',(-0.905967409625651,1.,1.52984849887993));
#27117=CARTESIAN_POINT('Ctrl Pts',(-0.899185047483511,1.,1.51805569590094));
#27118=CARTESIAN_POINT('Ctrl Pts',(-0.894452006964543,1.,1.50980486806688));
#27119=CARTESIAN_POINT('Ctrl Pts',(-0.892032620296855,1.,1.5055822144029));
#27120=CARTESIAN_POINT('',(-1.23627494547115,0.,1.81978687191668));
#27121=CARTESIAN_POINT('Origin',(-1.34869019493419,0.,1.73811241238545));
#27122=CARTESIAN_POINT('',(-1.34869019493419,1.,1.73811241238545));
#27123=CARTESIAN_POINT('',(-1.23627494547115,1.,1.81978687191668));
#27124=CARTESIAN_POINT('',(-1.34869019493419,0.,1.73811241238545));
#27125=CARTESIAN_POINT('Ctrl Pts',(-1.15624053661742,-1.,1.31362392696032));
#27126=CARTESIAN_POINT('Ctrl Pts',(-1.15624053661742,1.,1.31362392696032));
#27127=CARTESIAN_POINT('Ctrl Pts',(-1.15950888730809,-1.,1.31722977216397));
#27128=CARTESIAN_POINT('Ctrl Pts',(-1.15950888730809,1.,1.31722977216397));
#27129=CARTESIAN_POINT('Ctrl Pts',(-1.16589330093588,-1.,1.32428080721772));
#27130=CARTESIAN_POINT('Ctrl Pts',(-1.16589330093588,1.,1.32428080721772));
#27131=CARTESIAN_POINT('Ctrl Pts',(-1.17501305789857,-1.,1.33437539347008));
#27132=CARTESIAN_POINT('Ctrl Pts',(-1.17501305789857,1.,1.33437539347008));
#27133=CARTESIAN_POINT('Ctrl Pts',(-1.18625865667441,-1.,1.34687054001093));
#27134=CARTESIAN_POINT('Ctrl Pts',(-1.18625865667441,1.,1.34687054001093));
#27135=CARTESIAN_POINT('Ctrl Pts',(-1.1987959077932,-1.,1.36088705043885));
#27136=CARTESIAN_POINT('Ctrl Pts',(-1.1987959077932,1.,1.36088705043885));
#27137=CARTESIAN_POINT('Ctrl Pts',(-1.20982812925645,-1.,1.37331915607905));
#27138=CARTESIAN_POINT('Ctrl Pts',(-1.20982812925645,1.,1.37331915607905));
#27139=CARTESIAN_POINT('Ctrl Pts',(-1.21938737280852,-1.,1.38420564527715));
#27140=CARTESIAN_POINT('Ctrl Pts',(-1.21938737280852,1.,1.38420564527715));
#27141=CARTESIAN_POINT('Ctrl Pts',(-1.22752961899387,-1.,1.39361389568796));
#27142=CARTESIAN_POINT('Ctrl Pts',(-1.22752961899387,1.,1.39361389568796));
#27143=CARTESIAN_POINT('Ctrl Pts',(-1.23434087290423,-1.,1.40164708206106));
#27144=CARTESIAN_POINT('Ctrl Pts',(-1.23434087290423,1.,1.40164708206106));
#27145=CARTESIAN_POINT('Ctrl Pts',(-1.23994455029534,-1.,1.40845295531283));
#27146=CARTESIAN_POINT('Ctrl Pts',(-1.23994455029534,1.,1.40845295531283));
#27147=CARTESIAN_POINT('Ctrl Pts',(-1.24450600513056,-1.,1.41422913175179));
#27148=CARTESIAN_POINT('Ctrl Pts',(-1.24450600513056,1.,1.41422913175179));
#27149=CARTESIAN_POINT('Ctrl Pts',(-1.24824430986571,-1.,1.41923722596025));
#27150=CARTESIAN_POINT('Ctrl Pts',(-1.24824430986571,1.,1.41923722596025));
#27151=CARTESIAN_POINT('Ctrl Pts',(-1.2514145557001,-1.,1.42378102115575));
#27152=CARTESIAN_POINT('Ctrl Pts',(-1.2514145557001,1.,1.42378102115575));
#27153=CARTESIAN_POINT('Ctrl Pts',(-1.25426945222639,-1.,1.42815938799387));
#27154=CARTESIAN_POINT('Ctrl Pts',(-1.25426945222639,1.,1.42815938799387));
#27155=CARTESIAN_POINT('Ctrl Pts',(-1.25702687965755,-1.,1.43262645609691));
#27156=CARTESIAN_POINT('Ctrl Pts',(-1.25702687965755,1.,1.43262645609691));
#27157=CARTESIAN_POINT('Ctrl Pts',(-1.25983531012005,-1.,1.43734919180848));
#27158=CARTESIAN_POINT('Ctrl Pts',(-1.25983531012005,1.,1.43734919180848));
#27159=CARTESIAN_POINT('Ctrl Pts',(-1.26273903323859,-1.,1.44236470511303));
#27160=CARTESIAN_POINT('Ctrl Pts',(-1.26273903323859,1.,1.44236470511303));
#27161=CARTESIAN_POINT('Ctrl Pts',(-1.26570925118868,-1.,1.44761985001662));
#27162=CARTESIAN_POINT('Ctrl Pts',(-1.26570925118868,1.,1.44761985001662));
#27163=CARTESIAN_POINT('Ctrl Pts',(-1.2686778680489,-1.,1.45301422764247));
#27164=CARTESIAN_POINT('Ctrl Pts',(-1.2686778680489,1.,1.45301422764247));
#27165=CARTESIAN_POINT('Ctrl Pts',(-1.27156805265289,-1.,1.45843906294697));
#27166=CARTESIAN_POINT('Ctrl Pts',(-1.27156805265289,1.,1.45843906294697));
#27167=CARTESIAN_POINT('Ctrl Pts',(-1.27433119897822,-1.,1.46382431332476));
#27168=CARTESIAN_POINT('Ctrl Pts',(-1.27433119897822,1.,1.46382431332476));
#27169=CARTESIAN_POINT('Ctrl Pts',(-1.27696414831089,-1.,1.46916035917133));
#27170=CARTESIAN_POINT('Ctrl Pts',(-1.27696414831089,1.,1.46916035917133));
#27171=CARTESIAN_POINT('Ctrl Pts',(-1.2794891824849,-1.,1.4744717526707));
#27172=CARTESIAN_POINT('Ctrl Pts',(-1.2794891824849,1.,1.4744717526707));
#27173=CARTESIAN_POINT('Ctrl Pts',(-1.28194158939517,-1.,1.47980070347095));
#27174=CARTESIAN_POINT('Ctrl Pts',(-1.28194158939517,1.,1.47980070347095));
#27175=CARTESIAN_POINT('Ctrl Pts',(-1.28435533880201,-1.,1.4851881711891));
#27176=CARTESIAN_POINT('Ctrl Pts',(-1.28435533880201,1.,1.4851881711891));
#27177=CARTESIAN_POINT('Ctrl Pts',(-1.2867467611644,-1.,1.4906522831278));
#27178=CARTESIAN_POINT('Ctrl Pts',(-1.2867467611644,1.,1.4906522831278));
#27179=CARTESIAN_POINT('Ctrl Pts',(-1.28911506584254,-1.,1.49618896881754));
#27180=CARTESIAN_POINT('Ctrl Pts',(-1.28911506584254,1.,1.49618896881754));
#27181=CARTESIAN_POINT('Ctrl Pts',(-1.29145022885181,-1.,1.50178230149776));
#27182=CARTESIAN_POINT('Ctrl Pts',(-1.29145022885181,1.,1.50178230149776));
#27183=CARTESIAN_POINT('Ctrl Pts',(-1.29373841372842,-1.,1.50741159078365));
#27184=CARTESIAN_POINT('Ctrl Pts',(-1.29373841372842,1.,1.50741159078365));
#27185=CARTESIAN_POINT('Ctrl Pts',(-1.29596850710509,-1.,1.51305994241402));
#27186=CARTESIAN_POINT('Ctrl Pts',(-1.29596850710509,1.,1.51305994241402));
#27187=CARTESIAN_POINT('Ctrl Pts',(-1.29813791800747,-1.,1.51872184912724));
#27188=CARTESIAN_POINT('Ctrl Pts',(-1.29813791800747,1.,1.51872184912724));
#27189=CARTESIAN_POINT('Ctrl Pts',(-1.30024984366328,-1.,1.52439957861062));
#27190=CARTESIAN_POINT('Ctrl Pts',(-1.30024984366328,1.,1.52439957861062));
#27191=CARTESIAN_POINT('Ctrl Pts',(-1.30231064395568,-1.,1.53009970283891));
#27192=CARTESIAN_POINT('Ctrl Pts',(-1.30231064395568,1.,1.53009970283891));
#27193=CARTESIAN_POINT('Ctrl Pts',(-1.30432735639489,-1.,1.53582981268977));
#27194=CARTESIAN_POINT('Ctrl Pts',(-1.30432735639489,1.,1.53582981268977));
#27195=CARTESIAN_POINT('Ctrl Pts',(-1.30630475189556,-1.,1.54159462645432));
#27196=CARTESIAN_POINT('Ctrl Pts',(-1.30630475189556,1.,1.54159462645432));
#27197=CARTESIAN_POINT('Ctrl Pts',(-1.30824393907473,-1.,1.54739413957185));
#27198=CARTESIAN_POINT('Ctrl Pts',(-1.30824393907473,1.,1.54739413957185));
#27199=CARTESIAN_POINT('Ctrl Pts',(-1.31014393684222,-1.,1.55322568759481));
#27200=CARTESIAN_POINT('Ctrl Pts',(-1.31014393684222,1.,1.55322568759481));
#27201=CARTESIAN_POINT('Ctrl Pts',(-1.31200264341696,-1.,1.55908521254821));
#27202=CARTESIAN_POINT('Ctrl Pts',(-1.31200264341696,1.,1.55908521254821));
#27203=CARTESIAN_POINT('Ctrl Pts',(-1.31381795281002,-1.,1.56496872402353));
#27204=CARTESIAN_POINT('Ctrl Pts',(-1.31381795281002,1.,1.56496872402353));
#27205=CARTESIAN_POINT('Ctrl Pts',(-1.31558903860016,-1.,1.57087397835723));
#27206=CARTESIAN_POINT('Ctrl Pts',(-1.31558903860016,1.,1.57087397835723));
#27207=CARTESIAN_POINT('Ctrl Pts',(-1.31731642317187,-1.,1.5768005650559));
#27208=CARTESIAN_POINT('Ctrl Pts',(-1.31731642317187,1.,1.5768005650559));
#27209=CARTESIAN_POINT('Ctrl Pts',(-1.31900135021432,-1.,1.58274907898834));
#27210=CARTESIAN_POINT('Ctrl Pts',(-1.31900135021432,1.,1.58274907898834));
#27211=CARTESIAN_POINT('Ctrl Pts',(-1.32064537110892,-1.,1.58872057258245));
#27212=CARTESIAN_POINT('Ctrl Pts',(-1.32064537110892,1.,1.58872057258245));
#27213=CARTESIAN_POINT('Ctrl Pts',(-1.32224985747682,-1.,1.59471591079403));
#27214=CARTESIAN_POINT('Ctrl Pts',(-1.32224985747682,1.,1.59471591079403));
#27215=CARTESIAN_POINT('Ctrl Pts',(-1.32381550858256,-1.,1.60073511858687));
#27216=CARTESIAN_POINT('Ctrl Pts',(-1.32381550858256,1.,1.60073511858687));
#27217=CARTESIAN_POINT('Ctrl Pts',(-1.32534250785782,-1.,1.60677758290954));
#27218=CARTESIAN_POINT('Ctrl Pts',(-1.32534250785782,1.,1.60677758290954));
#27219=CARTESIAN_POINT('Ctrl Pts',(-1.32683074483356,-1.,1.6128423401575));
#27220=CARTESIAN_POINT('Ctrl Pts',(-1.32683074483356,1.,1.6128423401575));
#27221=CARTESIAN_POINT('Ctrl Pts',(-1.32828000610449,-1.,1.61892832270724));
#27222=CARTESIAN_POINT('Ctrl Pts',(-1.32828000610449,1.,1.61892832270724));
#27223=CARTESIAN_POINT('Ctrl Pts',(-1.3296901950568,-1.,1.62503464209797));
#27224=CARTESIAN_POINT('Ctrl Pts',(-1.3296901950568,1.,1.62503464209797));
#27225=CARTESIAN_POINT('Ctrl Pts',(-1.33106149345645,-1.,1.63116079730923));
#27226=CARTESIAN_POINT('Ctrl Pts',(-1.33106149345645,1.,1.63116079730923));
#27227=CARTESIAN_POINT('Ctrl Pts',(-1.33239425103724,-1.,1.63730653475089));
#27228=CARTESIAN_POINT('Ctrl Pts',(-1.33239425103724,1.,1.63730653475089));
#27229=CARTESIAN_POINT('Ctrl Pts',(-1.33368890676572,-1.,1.6434717485603));
#27230=CARTESIAN_POINT('Ctrl Pts',(-1.33368890676572,1.,1.6434717485603));
#27231=CARTESIAN_POINT('Ctrl Pts',(-1.33494590467993,-1.,1.6496563728683));
#27232=CARTESIAN_POINT('Ctrl Pts',(-1.33494590467993,1.,1.6496563728683));
#27233=CARTESIAN_POINT('Ctrl Pts',(-1.33616559745172,-1.,1.65586025952593));
#27234=CARTESIAN_POINT('Ctrl Pts',(-1.33616559745172,1.,1.65586025952593));
#27235=CARTESIAN_POINT('Ctrl Pts',(-1.33734820885262,-1.,1.66208312541983));
#27236=CARTESIAN_POINT('Ctrl Pts',(-1.33734820885262,1.,1.66208312541983));
#27237=CARTESIAN_POINT('Ctrl Pts',(-1.33849388654388,-1.,1.66832460783989));
#27238=CARTESIAN_POINT('Ctrl Pts',(-1.33849388654388,1.,1.66832460783989));
#27239=CARTESIAN_POINT('Ctrl Pts',(-1.3396027347034,-1.,1.67458429426086));
#27240=CARTESIAN_POINT('Ctrl Pts',(-1.3396027347034,1.,1.67458429426086));
#27241=CARTESIAN_POINT('Ctrl Pts',(-1.34067485185203,-1.,1.68086176030362));
#27242=CARTESIAN_POINT('Ctrl Pts',(-1.34067485185203,1.,1.68086176030362));
#27243=CARTESIAN_POINT('Ctrl Pts',(-1.341710374848,-1.,1.68715660868764));
#27244=CARTESIAN_POINT('Ctrl Pts',(-1.341710374848,1.,1.68715660868764));
#27245=CARTESIAN_POINT('Ctrl Pts',(-1.34270948206319,-1.,1.6934684849687));
#27246=CARTESIAN_POINT('Ctrl Pts',(-1.34270948206319,1.,1.6934684849687));
#27247=CARTESIAN_POINT('Ctrl Pts',(-1.34367237124483,-1.,1.69979707754427));
#27248=CARTESIAN_POINT('Ctrl Pts',(-1.34367237124483,1.,1.69979707754427));
#27249=CARTESIAN_POINT('Ctrl Pts',(-1.34459924533831,-1.,1.70614212266738));
#27250=CARTESIAN_POINT('Ctrl Pts',(-1.34459924533831,1.,1.70614212266738));
#27251=CARTESIAN_POINT('Ctrl Pts',(-1.34549029589416,-1.,1.71250340686822));
#27252=CARTESIAN_POINT('Ctrl Pts',(-1.34549029589416,1.,1.71250340686822));
#27253=CARTESIAN_POINT('Ctrl Pts',(-1.34634568653227,-1.,1.7188807715049));
#27254=CARTESIAN_POINT('Ctrl Pts',(-1.34634568653227,1.,1.7188807715049));
#27255=CARTESIAN_POINT('Ctrl Pts',(-1.34716554819527,-1.,1.72527410680674));
#27256=CARTESIAN_POINT('Ctrl Pts',(-1.34716554819527,1.,1.72527410680674));
#27257=CARTESIAN_POINT('Ctrl Pts',(-1.34779309152035,-1.,1.7304014965394));
#27258=CARTESIAN_POINT('Ctrl Pts',(-1.34779309152035,1.,1.7304014965394));
#27259=CARTESIAN_POINT('Ctrl Pts',(-1.34824783112887,-1.,1.73425417885907));
#27260=CARTESIAN_POINT('Ctrl Pts',(-1.34824783112887,1.,1.73425417885907));
#27261=CARTESIAN_POINT('Ctrl Pts',(-1.34854391898045,-1.,1.73682580585691));
#27262=CARTESIAN_POINT('Ctrl Pts',(-1.34854391898045,1.,1.73682580585691));
#27263=CARTESIAN_POINT('Ctrl Pts',(-1.34869019493419,-1.,1.73811241238545));
#27264=CARTESIAN_POINT('Ctrl Pts',(-1.34869019493419,1.,1.73811241238545));
#27265=CARTESIAN_POINT('',(-1.15624053661742,1.,1.31362392696032));
#27266=CARTESIAN_POINT('Ctrl Pts',(-1.15624053661742,1.,1.31362392696032));
#27267=CARTESIAN_POINT('Ctrl Pts',(-1.15950888730809,1.,1.31722977216397));
#27268=CARTESIAN_POINT('Ctrl Pts',(-1.16589330093588,1.,1.32428080721772));
#27269=CARTESIAN_POINT('Ctrl Pts',(-1.17501305789857,1.,1.33437539347008));
#27270=CARTESIAN_POINT('Ctrl Pts',(-1.18625865667441,1.,1.34687054001093));
#27271=CARTESIAN_POINT('Ctrl Pts',(-1.1987959077932,1.,1.36088705043885));
#27272=CARTESIAN_POINT('Ctrl Pts',(-1.20982812925645,1.,1.37331915607905));
#27273=CARTESIAN_POINT('Ctrl Pts',(-1.21938737280852,1.,1.38420564527715));
#27274=CARTESIAN_POINT('Ctrl Pts',(-1.22752961899387,1.,1.39361389568796));
#27275=CARTESIAN_POINT('Ctrl Pts',(-1.23434087290423,1.,1.40164708206106));
#27276=CARTESIAN_POINT('Ctrl Pts',(-1.23994455029534,1.,1.40845295531283));
#27277=CARTESIAN_POINT('Ctrl Pts',(-1.24450600513056,1.,1.41422913175179));
#27278=CARTESIAN_POINT('Ctrl Pts',(-1.24824430986571,1.,1.41923722596025));
#27279=CARTESIAN_POINT('Ctrl Pts',(-1.2514145557001,1.,1.42378102115575));
#27280=CARTESIAN_POINT('Ctrl Pts',(-1.25426945222639,1.,1.42815938799387));
#27281=CARTESIAN_POINT('Ctrl Pts',(-1.25702687965755,1.,1.43262645609691));
#27282=CARTESIAN_POINT('Ctrl Pts',(-1.25983531012005,1.,1.43734919180848));
#27283=CARTESIAN_POINT('Ctrl Pts',(-1.26273903323859,1.,1.44236470511303));
#27284=CARTESIAN_POINT('Ctrl Pts',(-1.26570925118868,1.,1.44761985001662));
#27285=CARTESIAN_POINT('Ctrl Pts',(-1.2686778680489,1.,1.45301422764247));
#27286=CARTESIAN_POINT('Ctrl Pts',(-1.27156805265289,1.,1.45843906294697));
#27287=CARTESIAN_POINT('Ctrl Pts',(-1.27433119897822,1.,1.46382431332476));
#27288=CARTESIAN_POINT('Ctrl Pts',(-1.27696414831089,1.,1.46916035917133));
#27289=CARTESIAN_POINT('Ctrl Pts',(-1.2794891824849,1.,1.4744717526707));
#27290=CARTESIAN_POINT('Ctrl Pts',(-1.28194158939517,1.,1.47980070347095));
#27291=CARTESIAN_POINT('Ctrl Pts',(-1.28435533880201,1.,1.4851881711891));
#27292=CARTESIAN_POINT('Ctrl Pts',(-1.2867467611644,1.,1.4906522831278));
#27293=CARTESIAN_POINT('Ctrl Pts',(-1.28911506584254,1.,1.49618896881754));
#27294=CARTESIAN_POINT('Ctrl Pts',(-1.29145022885181,1.,1.50178230149776));
#27295=CARTESIAN_POINT('Ctrl Pts',(-1.29373841372842,1.,1.50741159078365));
#27296=CARTESIAN_POINT('Ctrl Pts',(-1.29596850710509,1.,1.51305994241402));
#27297=CARTESIAN_POINT('Ctrl Pts',(-1.29813791800747,1.,1.51872184912724));
#27298=CARTESIAN_POINT('Ctrl Pts',(-1.30024984366328,1.,1.52439957861062));
#27299=CARTESIAN_POINT('Ctrl Pts',(-1.30231064395568,1.,1.53009970283891));
#27300=CARTESIAN_POINT('Ctrl Pts',(-1.30432735639489,1.,1.53582981268977));
#27301=CARTESIAN_POINT('Ctrl Pts',(-1.30630475189556,1.,1.54159462645432));
#27302=CARTESIAN_POINT('Ctrl Pts',(-1.30824393907473,1.,1.54739413957185));
#27303=CARTESIAN_POINT('Ctrl Pts',(-1.31014393684222,1.,1.55322568759481));
#27304=CARTESIAN_POINT('Ctrl Pts',(-1.31200264341696,1.,1.55908521254821));
#27305=CARTESIAN_POINT('Ctrl Pts',(-1.31381795281002,1.,1.56496872402353));
#27306=CARTESIAN_POINT('Ctrl Pts',(-1.31558903860016,1.,1.57087397835723));
#27307=CARTESIAN_POINT('Ctrl Pts',(-1.31731642317187,1.,1.5768005650559));
#27308=CARTESIAN_POINT('Ctrl Pts',(-1.31900135021432,1.,1.58274907898834));
#27309=CARTESIAN_POINT('Ctrl Pts',(-1.32064537110892,1.,1.58872057258245));
#27310=CARTESIAN_POINT('Ctrl Pts',(-1.32224985747682,1.,1.59471591079403));
#27311=CARTESIAN_POINT('Ctrl Pts',(-1.32381550858256,1.,1.60073511858687));
#27312=CARTESIAN_POINT('Ctrl Pts',(-1.32534250785782,1.,1.60677758290954));
#27313=CARTESIAN_POINT('Ctrl Pts',(-1.32683074483356,1.,1.6128423401575));
#27314=CARTESIAN_POINT('Ctrl Pts',(-1.32828000610449,1.,1.61892832270724));
#27315=CARTESIAN_POINT('Ctrl Pts',(-1.3296901950568,1.,1.62503464209797));
#27316=CARTESIAN_POINT('Ctrl Pts',(-1.33106149345645,1.,1.63116079730923));
#27317=CARTESIAN_POINT('Ctrl Pts',(-1.33239425103724,1.,1.63730653475089));
#27318=CARTESIAN_POINT('Ctrl Pts',(-1.33368890676572,1.,1.6434717485603));
#27319=CARTESIAN_POINT('Ctrl Pts',(-1.33494590467993,1.,1.6496563728683));
#27320=CARTESIAN_POINT('Ctrl Pts',(-1.33616559745172,1.,1.65586025952593));
#27321=CARTESIAN_POINT('Ctrl Pts',(-1.33734820885262,1.,1.66208312541983));
#27322=CARTESIAN_POINT('Ctrl Pts',(-1.33849388654388,1.,1.66832460783989));
#27323=CARTESIAN_POINT('Ctrl Pts',(-1.3396027347034,1.,1.67458429426086));
#27324=CARTESIAN_POINT('Ctrl Pts',(-1.34067485185203,1.,1.68086176030362));
#27325=CARTESIAN_POINT('Ctrl Pts',(-1.341710374848,1.,1.68715660868764));
#27326=CARTESIAN_POINT('Ctrl Pts',(-1.34270948206319,1.,1.6934684849687));
#27327=CARTESIAN_POINT('Ctrl Pts',(-1.34367237124483,1.,1.69979707754427));
#27328=CARTESIAN_POINT('Ctrl Pts',(-1.34459924533831,1.,1.70614212266738));
#27329=CARTESIAN_POINT('Ctrl Pts',(-1.34549029589416,1.,1.71250340686822));
#27330=CARTESIAN_POINT('Ctrl Pts',(-1.34634568653227,1.,1.7188807715049));
#27331=CARTESIAN_POINT('Ctrl Pts',(-1.34716554819527,1.,1.72527410680674));
#27332=CARTESIAN_POINT('Ctrl Pts',(-1.34779309152035,1.,1.7304014965394));
#27333=CARTESIAN_POINT('Ctrl Pts',(-1.34824783112887,1.,1.73425417885907));
#27334=CARTESIAN_POINT('Ctrl Pts',(-1.34854391898045,1.,1.73682580585691));
#27335=CARTESIAN_POINT('Ctrl Pts',(-1.34869019493419,1.,1.73811241238545));
#27336=CARTESIAN_POINT('',(-1.15624053661742,0.,1.31362392696032));
#27337=CARTESIAN_POINT('Origin',(0.,0.,0.));
#27338=CARTESIAN_POINT('',(-1.31362392696033,1.,1.15624053661742));
#27339=CARTESIAN_POINT('Origin',(0.,1.,0.));
#27340=CARTESIAN_POINT('',(-1.31362392696033,0.,1.15624053661742));
#27341=CARTESIAN_POINT('Ctrl Pts',(-1.73811241238545,-1.,1.34869019493419));
#27342=CARTESIAN_POINT('Ctrl Pts',(-1.73811241238545,1.,1.34869019493419));
#27343=CARTESIAN_POINT('Ctrl Pts',(-1.73682580585819,-1.,1.34854391898145));
#27344=CARTESIAN_POINT('Ctrl Pts',(-1.73682580585819,1.,1.34854391898145));
#27345=CARTESIAN_POINT('Ctrl Pts',(-1.73425417886255,-1.,1.34824783113158));
#27346=CARTESIAN_POINT('Ctrl Pts',(-1.73425417886255,1.,1.34824783113158));
#27347=CARTESIAN_POINT('Ctrl Pts',(-1.73040149654497,-1.,1.3477930915247));
#27348=CARTESIAN_POINT('Ctrl Pts',(-1.73040149654497,1.,1.3477930915247));
#27349=CARTESIAN_POINT('Ctrl Pts',(-1.72527410681298,-1.,1.34716554820013));
#27350=CARTESIAN_POINT('Ctrl Pts',(-1.72527410681298,1.,1.34716554820013));
#27351=CARTESIAN_POINT('Ctrl Pts',(-1.7188807715095,-1.,1.34634568653586));
#27352=CARTESIAN_POINT('Ctrl Pts',(-1.7188807715095,1.,1.34634568653586));
#27353=CARTESIAN_POINT('Ctrl Pts',(-1.71250340687011,-1.,1.34549029589563));
#27354=CARTESIAN_POINT('Ctrl Pts',(-1.71250340687011,1.,1.34549029589563));
#27355=CARTESIAN_POINT('Ctrl Pts',(-1.70614212266676,-1.,1.34459924533783));
#27356=CARTESIAN_POINT('Ctrl Pts',(-1.70614212266676,1.,1.34459924533783));
#27357=CARTESIAN_POINT('Ctrl Pts',(-1.69979707754221,-1.,1.34367237124322));
#27358=CARTESIAN_POINT('Ctrl Pts',(-1.69979707754221,1.,1.34367237124322));
#27359=CARTESIAN_POINT('Ctrl Pts',(-1.6934684849664,-1.,1.34270948206139));
#27360=CARTESIAN_POINT('Ctrl Pts',(-1.6934684849664,1.,1.34270948206139));
#27361=CARTESIAN_POINT('Ctrl Pts',(-1.68715660868602,-1.,1.34171037484673));
#27362=CARTESIAN_POINT('Ctrl Pts',(-1.68715660868602,1.,1.34171037484673));
#27363=CARTESIAN_POINT('Ctrl Pts',(-1.68086176030308,-1.,1.3406748518516));
#27364=CARTESIAN_POINT('Ctrl Pts',(-1.68086176030308,1.,1.3406748518516));
#27365=CARTESIAN_POINT('Ctrl Pts',(-1.67458429426126,-1.,1.33960273470372));
#27366=CARTESIAN_POINT('Ctrl Pts',(-1.67458429426126,1.,1.33960273470372));
#27367=CARTESIAN_POINT('Ctrl Pts',(-1.66832460784078,-1.,1.33849388654458));
#27368=CARTESIAN_POINT('Ctrl Pts',(-1.66832460784078,1.,1.33849388654458));
#27369=CARTESIAN_POINT('Ctrl Pts',(-1.66208312542073,-1.,1.33734820885331));
#27370=CARTESIAN_POINT('Ctrl Pts',(-1.66208312542073,1.,1.33734820885331));
#27371=CARTESIAN_POINT('Ctrl Pts',(-1.65586025952651,-1.,1.33616559745217));
#27372=CARTESIAN_POINT('Ctrl Pts',(-1.65586025952651,1.,1.33616559745217));
#27373=CARTESIAN_POINT('Ctrl Pts',(-1.64965637286843,-1.,1.33494590468003));
#27374=CARTESIAN_POINT('Ctrl Pts',(-1.64965637286843,1.,1.33494590468003));
#27375=CARTESIAN_POINT('Ctrl Pts',(-1.64347174856007,-1.,1.33368890676554));
#27376=CARTESIAN_POINT('Ctrl Pts',(-1.64347174856007,1.,1.33368890676554));
#27377=CARTESIAN_POINT('Ctrl Pts',(-1.6373065347505,-1.,1.33239425103694));
#27378=CARTESIAN_POINT('Ctrl Pts',(-1.6373065347505,1.,1.33239425103694));
#27379=CARTESIAN_POINT('Ctrl Pts',(-1.63116079730887,-1.,1.33106149345618));
#27380=CARTESIAN_POINT('Ctrl Pts',(-1.63116079730887,1.,1.33106149345618));
#27381=CARTESIAN_POINT('Ctrl Pts',(-1.62503464209777,-1.,1.32969019505665));
#27382=CARTESIAN_POINT('Ctrl Pts',(-1.62503464209777,1.,1.32969019505665));
#27383=CARTESIAN_POINT('Ctrl Pts',(-1.61892832270723,-1.,1.32828000610448));
#27384=CARTESIAN_POINT('Ctrl Pts',(-1.61892832270723,1.,1.32828000610448));
#27385=CARTESIAN_POINT('Ctrl Pts',(-1.61284234015762,-1.,1.32683074483365));
#27386=CARTESIAN_POINT('Ctrl Pts',(-1.61284234015762,1.,1.32683074483365));
#27387=CARTESIAN_POINT('Ctrl Pts',(-1.6067775829097,-1.,1.32534250785794));
#27388=CARTESIAN_POINT('Ctrl Pts',(-1.6067775829097,1.,1.32534250785794));
#27389=CARTESIAN_POINT('Ctrl Pts',(-1.600735118587,-1.,1.32381550858266));
#27390=CARTESIAN_POINT('Ctrl Pts',(-1.600735118587,1.,1.32381550858266));
#27391=CARTESIAN_POINT('Ctrl Pts',(-1.59471591079408,-1.,1.32224985747686));
#27392=CARTESIAN_POINT('Ctrl Pts',(-1.59471591079408,1.,1.32224985747686));
#27393=CARTESIAN_POINT('Ctrl Pts',(-1.58872057258244,-1.,1.32064537110891));
#27394=CARTESIAN_POINT('Ctrl Pts',(-1.58872057258244,1.,1.32064537110891));
#27395=CARTESIAN_POINT('Ctrl Pts',(-1.58274907898829,-1.,1.31900135021428));
#27396=CARTESIAN_POINT('Ctrl Pts',(-1.58274907898829,1.,1.31900135021428));
#27397=CARTESIAN_POINT('Ctrl Pts',(-1.57680056505585,-1.,1.31731642317183));
#27398=CARTESIAN_POINT('Ctrl Pts',(-1.57680056505585,1.,1.31731642317183));
#27399=CARTESIAN_POINT('Ctrl Pts',(-1.57087397835721,-1.,1.31558903860015));
#27400=CARTESIAN_POINT('Ctrl Pts',(-1.57087397835721,1.,1.31558903860015));
#27401=CARTESIAN_POINT('Ctrl Pts',(-1.56496872402352,-1.,1.31381795281002));
#27402=CARTESIAN_POINT('Ctrl Pts',(-1.56496872402352,1.,1.31381795281002));
#27403=CARTESIAN_POINT('Ctrl Pts',(-1.55908521254822,-1.,1.31200264341696));
#27404=CARTESIAN_POINT('Ctrl Pts',(-1.55908521254822,1.,1.31200264341696));
#27405=CARTESIAN_POINT('Ctrl Pts',(-1.55322568759481,-1.,1.31014393684221));
#27406=CARTESIAN_POINT('Ctrl Pts',(-1.55322568759481,1.,1.31014393684221));
#27407=CARTESIAN_POINT('Ctrl Pts',(-1.54739413957183,-1.,1.30824393907471));
#27408=CARTESIAN_POINT('Ctrl Pts',(-1.54739413957183,1.,1.30824393907471));
#27409=CARTESIAN_POINT('Ctrl Pts',(-1.54159462645428,-1.,1.30630475189553));
#27410=CARTESIAN_POINT('Ctrl Pts',(-1.54159462645428,1.,1.30630475189553));
#27411=CARTESIAN_POINT('Ctrl Pts',(-1.53582981268976,-1.,1.30432735639487));
#27412=CARTESIAN_POINT('Ctrl Pts',(-1.53582981268976,1.,1.30432735639487));
#27413=CARTESIAN_POINT('Ctrl Pts',(-1.53009970283893,-1.,1.3023106439557));
#27414=CARTESIAN_POINT('Ctrl Pts',(-1.53009970283893,1.,1.3023106439557));
#27415=CARTESIAN_POINT('Ctrl Pts',(-1.5243995786107,-1.,1.30024984366334));
#27416=CARTESIAN_POINT('Ctrl Pts',(-1.5243995786107,1.,1.30024984366334));
#27417=CARTESIAN_POINT('Ctrl Pts',(-1.51872184912735,-1.,1.29813791800757));
#27418=CARTESIAN_POINT('Ctrl Pts',(-1.51872184912735,1.,1.29813791800757));
#27419=CARTESIAN_POINT('Ctrl Pts',(-1.51305994241412,-1.,1.29596850710518));
#27420=CARTESIAN_POINT('Ctrl Pts',(-1.51305994241412,1.,1.29596850710518));
#27421=CARTESIAN_POINT('Ctrl Pts',(-1.50741159078367,-1.,1.29373841372843));
#27422=CARTESIAN_POINT('Ctrl Pts',(-1.50741159078367,1.,1.29373841372843));
#27423=CARTESIAN_POINT('Ctrl Pts',(-1.50178230149764,-1.,1.29145022885171));
#27424=CARTESIAN_POINT('Ctrl Pts',(-1.50178230149764,1.,1.29145022885171));
#27425=CARTESIAN_POINT('Ctrl Pts',(-1.49618896881729,-1.,1.28911506584232));
#27426=CARTESIAN_POINT('Ctrl Pts',(-1.49618896881729,1.,1.28911506584232));
#27427=CARTESIAN_POINT('Ctrl Pts',(-1.4906522831275,-1.,1.28674676116415));
#27428=CARTESIAN_POINT('Ctrl Pts',(-1.4906522831275,1.,1.28674676116415));
#27429=CARTESIAN_POINT('Ctrl Pts',(-1.48518817118891,-1.,1.28435533880184));
#27430=CARTESIAN_POINT('Ctrl Pts',(-1.48518817118891,1.,1.28435533880184));
#27431=CARTESIAN_POINT('Ctrl Pts',(-1.47980070347102,-1.,1.28194158939522));
#27432=CARTESIAN_POINT('Ctrl Pts',(-1.47980070347102,1.,1.28194158939522));
#27433=CARTESIAN_POINT('Ctrl Pts',(-1.4744717526711,-1.,1.27948918248524));
#27434=CARTESIAN_POINT('Ctrl Pts',(-1.4744717526711,1.,1.27948918248524));
#27435=CARTESIAN_POINT('Ctrl Pts',(-1.46916035917197,-1.,1.27696414831144));
#27436=CARTESIAN_POINT('Ctrl Pts',(-1.46916035917197,1.,1.27696414831144));
#27437=CARTESIAN_POINT('Ctrl Pts',(-1.4638243133254,-1.,1.27433119897877));
#27438=CARTESIAN_POINT('Ctrl Pts',(-1.4638243133254,1.,1.27433119897877));
#27439=CARTESIAN_POINT('Ctrl Pts',(-1.45843906294725,-1.,1.27156805265312));
#27440=CARTESIAN_POINT('Ctrl Pts',(-1.45843906294725,1.,1.27156805265312));
#27441=CARTESIAN_POINT('Ctrl Pts',(-1.45301422764205,-1.,1.26867786804854));
#27442=CARTESIAN_POINT('Ctrl Pts',(-1.45301422764205,1.,1.26867786804854));
#27443=CARTESIAN_POINT('Ctrl Pts',(-1.44761985001544,-1.,1.26570925118767));
#27444=CARTESIAN_POINT('Ctrl Pts',(-1.44761985001544,1.,1.26570925118767));
#27445=CARTESIAN_POINT('Ctrl Pts',(-1.44236470511145,-1.,1.26273903323723));
#27446=CARTESIAN_POINT('Ctrl Pts',(-1.44236470511145,1.,1.26273903323723));
#27447=CARTESIAN_POINT('Ctrl Pts',(-1.43734919180719,-1.,1.25983531011894));
#27448=CARTESIAN_POINT('Ctrl Pts',(-1.43734919180719,1.,1.25983531011894));
#27449=CARTESIAN_POINT('Ctrl Pts',(-1.43262645609679,-1.,1.25702687965744));
#27450=CARTESIAN_POINT('Ctrl Pts',(-1.43262645609679,1.,1.25702687965744));
#27451=CARTESIAN_POINT('Ctrl Pts',(-1.42815938799555,-1.,1.25426945222783));
#27452=CARTESIAN_POINT('Ctrl Pts',(-1.42815938799555,1.,1.25426945222783));
#27453=CARTESIAN_POINT('Ctrl Pts',(-1.42378102115911,-1.,1.25141455570299));
#27454=CARTESIAN_POINT('Ctrl Pts',(-1.42378102115911,1.,1.25141455570299));
#27455=CARTESIAN_POINT('Ctrl Pts',(-1.41923722596421,-1.,1.24824430986911));
#27456=CARTESIAN_POINT('Ctrl Pts',(-1.41923722596421,1.,1.24824430986911));
#27457=CARTESIAN_POINT('Ctrl Pts',(-1.41422913175437,-1.,1.24450600513278));
#27458=CARTESIAN_POINT('Ctrl Pts',(-1.41422913175437,1.,1.24450600513278));
#27459=CARTESIAN_POINT('Ctrl Pts',(-1.40845295531151,-1.,1.23994455029421));
#27460=CARTESIAN_POINT('Ctrl Pts',(-1.40845295531151,1.,1.23994455029421));
#27461=CARTESIAN_POINT('Ctrl Pts',(-1.40164708205345,-1.,1.23434087289768));
#27462=CARTESIAN_POINT('Ctrl Pts',(-1.40164708205345,1.,1.23434087289768));
#27463=CARTESIAN_POINT('Ctrl Pts',(-1.39361389567257,-1.,1.22752961898063));
#27464=CARTESIAN_POINT('Ctrl Pts',(-1.39361389567257,1.,1.22752961898063));
#27465=CARTESIAN_POINT('Ctrl Pts',(-1.38420564525391,-1.,1.21938737278853));
#27466=CARTESIAN_POINT('Ctrl Pts',(-1.38420564525391,1.,1.21938737278853));
#27467=CARTESIAN_POINT('Ctrl Pts',(-1.37331915604962,-1.,1.20982812923113));
#27468=CARTESIAN_POINT('Ctrl Pts',(-1.37331915604962,1.,1.20982812923113));
#27469=CARTESIAN_POINT('Ctrl Pts',(-1.36088705040677,-1.,1.1987959077656));
#27470=CARTESIAN_POINT('Ctrl Pts',(-1.36088705040677,1.,1.1987959077656));
#27471=CARTESIAN_POINT('Ctrl Pts',(-1.34687053998157,-1.,1.18625865664915));
#27472=CARTESIAN_POINT('Ctrl Pts',(-1.34687053998157,1.,1.18625865664915));
#27473=CARTESIAN_POINT('Ctrl Pts',(-1.33437539344842,-1.,1.17501305787994));
#27474=CARTESIAN_POINT('Ctrl Pts',(-1.33437539344842,1.,1.17501305787994));
#27475=CARTESIAN_POINT('Ctrl Pts',(-1.32428080720544,-1.,1.16589330092532));
#27476=CARTESIAN_POINT('Ctrl Pts',(-1.32428080720544,1.,1.16589330092532));
#27477=CARTESIAN_POINT('Ctrl Pts',(-1.3172297721596,-1.,1.15950888730433));
#27478=CARTESIAN_POINT('Ctrl Pts',(-1.3172297721596,1.,1.15950888730433));
#27479=CARTESIAN_POINT('Ctrl Pts',(-1.31362392696033,-1.,1.15624053661742));
#27480=CARTESIAN_POINT('Ctrl Pts',(-1.31362392696033,1.,1.15624053661742));
#27481=CARTESIAN_POINT('',(-1.73811241238545,1.,1.34869019493419));
#27482=CARTESIAN_POINT('Ctrl Pts',(-1.73811241238545,1.,1.34869019493419));
#27483=CARTESIAN_POINT('Ctrl Pts',(-1.73682580585819,1.,1.34854391898145));
#27484=CARTESIAN_POINT('Ctrl Pts',(-1.73425417886255,1.,1.34824783113158));
#27485=CARTESIAN_POINT('Ctrl Pts',(-1.73040149654497,1.,1.3477930915247));
#27486=CARTESIAN_POINT('Ctrl Pts',(-1.72527410681298,1.,1.34716554820013));
#27487=CARTESIAN_POINT('Ctrl Pts',(-1.7188807715095,1.,1.34634568653586));
#27488=CARTESIAN_POINT('Ctrl Pts',(-1.71250340687011,1.,1.34549029589563));
#27489=CARTESIAN_POINT('Ctrl Pts',(-1.70614212266676,1.,1.34459924533783));
#27490=CARTESIAN_POINT('Ctrl Pts',(-1.69979707754221,1.,1.34367237124322));
#27491=CARTESIAN_POINT('Ctrl Pts',(-1.6934684849664,1.,1.34270948206139));
#27492=CARTESIAN_POINT('Ctrl Pts',(-1.68715660868602,1.,1.34171037484673));
#27493=CARTESIAN_POINT('Ctrl Pts',(-1.68086176030308,1.,1.3406748518516));
#27494=CARTESIAN_POINT('Ctrl Pts',(-1.67458429426126,1.,1.33960273470372));
#27495=CARTESIAN_POINT('Ctrl Pts',(-1.66832460784078,1.,1.33849388654458));
#27496=CARTESIAN_POINT('Ctrl Pts',(-1.66208312542073,1.,1.33734820885331));
#27497=CARTESIAN_POINT('Ctrl Pts',(-1.65586025952651,1.,1.33616559745217));
#27498=CARTESIAN_POINT('Ctrl Pts',(-1.64965637286843,1.,1.33494590468003));
#27499=CARTESIAN_POINT('Ctrl Pts',(-1.64347174856007,1.,1.33368890676554));
#27500=CARTESIAN_POINT('Ctrl Pts',(-1.6373065347505,1.,1.33239425103694));
#27501=CARTESIAN_POINT('Ctrl Pts',(-1.63116079730887,1.,1.33106149345618));
#27502=CARTESIAN_POINT('Ctrl Pts',(-1.62503464209777,1.,1.32969019505665));
#27503=CARTESIAN_POINT('Ctrl Pts',(-1.61892832270723,1.,1.32828000610448));
#27504=CARTESIAN_POINT('Ctrl Pts',(-1.61284234015762,1.,1.32683074483365));
#27505=CARTESIAN_POINT('Ctrl Pts',(-1.6067775829097,1.,1.32534250785794));
#27506=CARTESIAN_POINT('Ctrl Pts',(-1.600735118587,1.,1.32381550858266));
#27507=CARTESIAN_POINT('Ctrl Pts',(-1.59471591079408,1.,1.32224985747686));
#27508=CARTESIAN_POINT('Ctrl Pts',(-1.58872057258244,1.,1.32064537110891));
#27509=CARTESIAN_POINT('Ctrl Pts',(-1.58274907898829,1.,1.31900135021428));
#27510=CARTESIAN_POINT('Ctrl Pts',(-1.57680056505585,1.,1.31731642317183));
#27511=CARTESIAN_POINT('Ctrl Pts',(-1.57087397835721,1.,1.31558903860015));
#27512=CARTESIAN_POINT('Ctrl Pts',(-1.56496872402352,1.,1.31381795281002));
#27513=CARTESIAN_POINT('Ctrl Pts',(-1.55908521254822,1.,1.31200264341696));
#27514=CARTESIAN_POINT('Ctrl Pts',(-1.55322568759481,1.,1.31014393684221));
#27515=CARTESIAN_POINT('Ctrl Pts',(-1.54739413957183,1.,1.30824393907471));
#27516=CARTESIAN_POINT('Ctrl Pts',(-1.54159462645428,1.,1.30630475189553));
#27517=CARTESIAN_POINT('Ctrl Pts',(-1.53582981268976,1.,1.30432735639487));
#27518=CARTESIAN_POINT('Ctrl Pts',(-1.53009970283893,1.,1.3023106439557));
#27519=CARTESIAN_POINT('Ctrl Pts',(-1.5243995786107,1.,1.30024984366334));
#27520=CARTESIAN_POINT('Ctrl Pts',(-1.51872184912735,1.,1.29813791800757));
#27521=CARTESIAN_POINT('Ctrl Pts',(-1.51305994241412,1.,1.29596850710518));
#27522=CARTESIAN_POINT('Ctrl Pts',(-1.50741159078367,1.,1.29373841372843));
#27523=CARTESIAN_POINT('Ctrl Pts',(-1.50178230149764,1.,1.29145022885171));
#27524=CARTESIAN_POINT('Ctrl Pts',(-1.49618896881729,1.,1.28911506584232));
#27525=CARTESIAN_POINT('Ctrl Pts',(-1.4906522831275,1.,1.28674676116415));
#27526=CARTESIAN_POINT('Ctrl Pts',(-1.48518817118891,1.,1.28435533880184));
#27527=CARTESIAN_POINT('Ctrl Pts',(-1.47980070347102,1.,1.28194158939522));
#27528=CARTESIAN_POINT('Ctrl Pts',(-1.4744717526711,1.,1.27948918248524));
#27529=CARTESIAN_POINT('Ctrl Pts',(-1.46916035917197,1.,1.27696414831144));
#27530=CARTESIAN_POINT('Ctrl Pts',(-1.4638243133254,1.,1.27433119897877));
#27531=CARTESIAN_POINT('Ctrl Pts',(-1.45843906294725,1.,1.27156805265312));
#27532=CARTESIAN_POINT('Ctrl Pts',(-1.45301422764205,1.,1.26867786804854));
#27533=CARTESIAN_POINT('Ctrl Pts',(-1.44761985001544,1.,1.26570925118767));
#27534=CARTESIAN_POINT('Ctrl Pts',(-1.44236470511145,1.,1.26273903323723));
#27535=CARTESIAN_POINT('Ctrl Pts',(-1.43734919180719,1.,1.25983531011894));
#27536=CARTESIAN_POINT('Ctrl Pts',(-1.43262645609679,1.,1.25702687965744));
#27537=CARTESIAN_POINT('Ctrl Pts',(-1.42815938799555,1.,1.25426945222783));
#27538=CARTESIAN_POINT('Ctrl Pts',(-1.42378102115911,1.,1.25141455570299));
#27539=CARTESIAN_POINT('Ctrl Pts',(-1.41923722596421,1.,1.24824430986911));
#27540=CARTESIAN_POINT('Ctrl Pts',(-1.41422913175437,1.,1.24450600513278));
#27541=CARTESIAN_POINT('Ctrl Pts',(-1.40845295531151,1.,1.23994455029421));
#27542=CARTESIAN_POINT('Ctrl Pts',(-1.40164708205345,1.,1.23434087289768));
#27543=CARTESIAN_POINT('Ctrl Pts',(-1.39361389567257,1.,1.22752961898063));
#27544=CARTESIAN_POINT('Ctrl Pts',(-1.38420564525391,1.,1.21938737278853));
#27545=CARTESIAN_POINT('Ctrl Pts',(-1.37331915604962,1.,1.20982812923113));
#27546=CARTESIAN_POINT('Ctrl Pts',(-1.36088705040677,1.,1.1987959077656));
#27547=CARTESIAN_POINT('Ctrl Pts',(-1.34687053998157,1.,1.18625865664915));
#27548=CARTESIAN_POINT('Ctrl Pts',(-1.33437539344842,1.,1.17501305787994));
#27549=CARTESIAN_POINT('Ctrl Pts',(-1.32428080720544,1.,1.16589330092532));
#27550=CARTESIAN_POINT('Ctrl Pts',(-1.3172297721596,1.,1.15950888730433));
#27551=CARTESIAN_POINT('Ctrl Pts',(-1.31362392696033,1.,1.15624053661742));
#27552=CARTESIAN_POINT('',(-1.73811241238545,0.,1.34869019493419));
#27553=CARTESIAN_POINT('Origin',(-1.81978687191668,0.,1.23627494547115));
#27554=CARTESIAN_POINT('',(-1.81978687191668,1.,1.23627494547115));
#27555=CARTESIAN_POINT('',(-1.73811241238545,1.,1.34869019493419));
#27556=CARTESIAN_POINT('',(-1.81978687191668,0.,1.23627494547115));
#27557=CARTESIAN_POINT('Ctrl Pts',(-1.5055822144029,-1.,0.892032620296855));
#27558=CARTESIAN_POINT('Ctrl Pts',(-1.5055822144029,1.,0.892032620296855));
#27559=CARTESIAN_POINT('Ctrl Pts',(-1.50980486807181,-1.,0.894452006967538));
#27560=CARTESIAN_POINT('Ctrl Pts',(-1.50980486807181,1.,0.894452006967538));
#27561=CARTESIAN_POINT('Ctrl Pts',(-1.51805569591479,-1.,0.89918504749193));
#27562=CARTESIAN_POINT('Ctrl Pts',(-1.51805569591479,1.,0.89918504749193));
#27563=CARTESIAN_POINT('Ctrl Pts',(-1.52984849890434,-1.,0.905967409640499));
#27564=CARTESIAN_POINT('Ctrl Pts',(-1.52984849890434,1.,0.905967409640499));
#27565=CARTESIAN_POINT('Ctrl Pts',(-1.54440491152808,-1.,0.91437591904658));
#27566=CARTESIAN_POINT('Ctrl Pts',(-1.54440491152808,1.,0.91437591904658));
#27567=CARTESIAN_POINT('Ctrl Pts',(-1.56065988582509,-1.,0.923832188966322));
#27568=CARTESIAN_POINT('Ctrl Pts',(-1.56065988582509,1.,0.923832188966322));
#27569=CARTESIAN_POINT('Ctrl Pts',(-1.57499388385561,-1.,0.932246680128849));
#27570=CARTESIAN_POINT('Ctrl Pts',(-1.57499388385561,1.,0.932246680128849));
#27571=CARTESIAN_POINT('Ctrl Pts',(-1.58744937489796,-1.,0.939646377909319));
#27572=CARTESIAN_POINT('Ctrl Pts',(-1.58744937489796,1.,0.939646377909319));
#27573=CARTESIAN_POINT('Ctrl Pts',(-1.59810042045408,-1.,0.946078063325796));
#27574=CARTESIAN_POINT('Ctrl Pts',(-1.59810042045408,1.,0.946078063325796));
#27575=CARTESIAN_POINT('Ctrl Pts',(-1.60706069897794,-1.,0.951613284361248));
#27576=CARTESIAN_POINT('Ctrl Pts',(-1.60706069897794,1.,0.951613284361248));
#27577=CARTESIAN_POINT('Ctrl Pts',(-1.61449324337233,-1.,0.956354422921573));
#27578=CARTESIAN_POINT('Ctrl Pts',(-1.61449324337233,1.,0.956354422921573));
#27579=CARTESIAN_POINT('Ctrl Pts',(-1.62061638139929,-1.,0.960438326099958));
#27580=CARTESIAN_POINT('Ctrl Pts',(-1.62061638139929,1.,0.960438326099958));
#27581=CARTESIAN_POINT('Ctrl Pts',(-1.6257193066974,-1.,0.964046107037821));
#27582=CARTESIAN_POINT('Ctrl Pts',(-1.6257193066974,1.,0.964046107037821));
#27583=CARTESIAN_POINT('Ctrl Pts',(-1.63013849959083,-1.,0.967387853228041));
#27584=CARTESIAN_POINT('Ctrl Pts',(-1.63013849959083,1.,0.967387853228041));
#27585=CARTESIAN_POINT('Ctrl Pts',(-1.63420665729609,-1.,0.970669715996356));
#27586=CARTESIAN_POINT('Ctrl Pts',(-1.63420665729609,1.,0.970669715996356));
#27587=CARTESIAN_POINT('Ctrl Pts',(-1.63820952658157,-1.,0.974066058287501));
#27588=CARTESIAN_POINT('Ctrl Pts',(-1.63820952658157,1.,0.974066058287501));
#27589=CARTESIAN_POINT('Ctrl Pts',(-1.64233990826831,-1.,0.977689794120297));
#27590=CARTESIAN_POINT('Ctrl Pts',(-1.64233990826831,1.,0.977689794120297));
#27591=CARTESIAN_POINT('Ctrl Pts',(-1.64665139190834,-1.,0.981562530940574));
#27592=CARTESIAN_POINT('Ctrl Pts',(-1.64665139190834,1.,0.981562530940574));
#27593=CARTESIAN_POINT('Ctrl Pts',(-1.6511001661277,-1.,0.985642622921626));
#27594=CARTESIAN_POINT('Ctrl Pts',(-1.6511001661277,1.,0.985642622921626));
#27595=CARTESIAN_POINT('Ctrl Pts',(-1.65559044289746,-1.,0.98985562785445));
#27596=CARTESIAN_POINT('Ctrl Pts',(-1.65559044289746,1.,0.98985562785445));
#27597=CARTESIAN_POINT('Ctrl Pts',(-1.66001553809916,-1.,0.994121836661116));
#27598=CARTESIAN_POINT('Ctrl Pts',(-1.66001553809916,1.,0.994121836661116));
#27599=CARTESIAN_POINT('Ctrl Pts',(-1.66430758030304,-1.,0.998389654952317));
#27600=CARTESIAN_POINT('Ctrl Pts',(-1.66430758030304,1.,0.998389654952317));
#27601=CARTESIAN_POINT('Ctrl Pts',(-1.66846059277231,-1.,1.00265091003682));
#27602=CARTESIAN_POINT('Ctrl Pts',(-1.66846059277231,1.,1.00265091003682));
#27603=CARTESIAN_POINT('Ctrl Pts',(-1.67250335383248,-1.,1.00692206696387));
#27604=CARTESIAN_POINT('Ctrl Pts',(-1.67250335383248,1.,1.00692206696387));
#27605=CARTESIAN_POINT('Ctrl Pts',(-1.67648246776457,-1.,1.01123236493507));
#27606=CARTESIAN_POINT('Ctrl Pts',(-1.67648246776457,1.,1.01123236493507));
#27607=CARTESIAN_POINT('Ctrl Pts',(-1.6804428989482,-1.,1.01561026162787));
#27608=CARTESIAN_POINT('Ctrl Pts',(-1.6804428989482,1.,1.01561026162787));
#27609=CARTESIAN_POINT('Ctrl Pts',(-1.68440578021739,-1.,1.02006795074222));
#27610=CARTESIAN_POINT('Ctrl Pts',(-1.68440578021739,1.,1.02006795074222));
#27611=CARTESIAN_POINT('Ctrl Pts',(-1.68836910178475,-1.,1.02460180535272));
#27612=CARTESIAN_POINT('Ctrl Pts',(-1.68836910178475,1.,1.02460180535272));
#27613=CARTESIAN_POINT('Ctrl Pts',(-1.69231840863471,-1.,1.02919977579155));
#27614=CARTESIAN_POINT('Ctrl Pts',(-1.69231840863471,1.,1.02919977579155));
#27615=CARTESIAN_POINT('Ctrl Pts',(-1.69623414782769,-1.,1.03384646003587));
#27616=CARTESIAN_POINT('Ctrl Pts',(-1.69623414782769,1.,1.03384646003587));
#27617=CARTESIAN_POINT('Ctrl Pts',(-1.70010052930951,-1.,1.03852922490782));
#27618=CARTESIAN_POINT('Ctrl Pts',(-1.70010052930951,1.,1.03852922490782));
#27619=CARTESIAN_POINT('Ctrl Pts',(-1.70391338707969,-1.,1.04324363334546));
#27620=CARTESIAN_POINT('Ctrl Pts',(-1.70391338707969,1.,1.04324363334546));
#27621=CARTESIAN_POINT('Ctrl Pts',(-1.70767646263641,-1.,1.0479908540499));
#27622=CARTESIAN_POINT('Ctrl Pts',(-1.70767646263641,1.,1.0479908540499));
#27623=CARTESIAN_POINT('Ctrl Pts',(-1.71139783543986,-1.,1.05277517202854));
#27624=CARTESIAN_POINT('Ctrl Pts',(-1.71139783543986,1.,1.05277517202854));
#27625=CARTESIAN_POINT('Ctrl Pts',(-1.71508654427022,-1.,1.05760163192481));
#27626=CARTESIAN_POINT('Ctrl Pts',(-1.71508654427022,1.,1.05760163192481));
#27627=CARTESIAN_POINT('Ctrl Pts',(-1.71874858456908,-1.,1.0624732468065));
#27628=CARTESIAN_POINT('Ctrl Pts',(-1.71874858456908,1.,1.0624732468065));
#27629=CARTESIAN_POINT('Ctrl Pts',(-1.72238500928456,-1.,1.06738966975463));
#27630=CARTESIAN_POINT('Ctrl Pts',(-1.72238500928456,1.,1.06738966975463));
#27631=CARTESIAN_POINT('Ctrl Pts',(-1.72599406198489,-1.,1.07234866990252));
#27632=CARTESIAN_POINT('Ctrl Pts',(-1.72599406198489,1.,1.07234866990252));
#27633=CARTESIAN_POINT('Ctrl Pts',(-1.72957248977424,-1.,1.0773470373727));
#27634=CARTESIAN_POINT('Ctrl Pts',(-1.72957248977424,1.,1.0773470373727));
#27635=CARTESIAN_POINT('Ctrl Pts',(-1.73311705663407,-1.,1.08238162784749));
#27636=CARTESIAN_POINT('Ctrl Pts',(-1.73311705663407,1.,1.08238162784749));
#27637=CARTESIAN_POINT('Ctrl Pts',(-1.73662628326093,-1.,1.08745056285429));
#27638=CARTESIAN_POINT('Ctrl Pts',(-1.73662628326093,1.,1.08745056285429));
#27639=CARTESIAN_POINT('Ctrl Pts',(-1.74010053962252,-1.,1.09255329056496));
#27640=CARTESIAN_POINT('Ctrl Pts',(-1.74010053962252,1.,1.09255329056496));
#27641=CARTESIAN_POINT('Ctrl Pts',(-1.74354119236212,-1.,1.09768999241229));
#27642=CARTESIAN_POINT('Ctrl Pts',(-1.74354119236212,1.,1.09768999241229));
#27643=CARTESIAN_POINT('Ctrl Pts',(-1.74695004214924,-1.,1.10286118991144));
#27644=CARTESIAN_POINT('Ctrl Pts',(-1.74695004214924,1.,1.10286118991144));
#27645=CARTESIAN_POINT('Ctrl Pts',(-1.75032866075914,-1.,1.10806728183003));
#27646=CARTESIAN_POINT('Ctrl Pts',(-1.75032866075914,1.,1.10806728183003));
#27647=CARTESIAN_POINT('Ctrl Pts',(-1.75367772094617,-1.,1.11330807582542));
#27648=CARTESIAN_POINT('Ctrl Pts',(-1.75367772094617,1.,1.11330807582542));
#27649=CARTESIAN_POINT('Ctrl Pts',(-1.75699720772089,-1.,1.11858293216752));
#27650=CARTESIAN_POINT('Ctrl Pts',(-1.75699720772089,1.,1.11858293216752));
#27651=CARTESIAN_POINT('Ctrl Pts',(-1.76028671825084,-1.,1.12389096855078));
#27652=CARTESIAN_POINT('Ctrl Pts',(-1.76028671825084,1.,1.12389096855078));
#27653=CARTESIAN_POINT('Ctrl Pts',(-1.76354571966171,-1.,1.12923123555076));
#27654=CARTESIAN_POINT('Ctrl Pts',(-1.76354571966171,1.,1.12923123555076));
#27655=CARTESIAN_POINT('Ctrl Pts',(-1.76677384551883,-1.,1.13460291804635));
#27656=CARTESIAN_POINT('Ctrl Pts',(-1.76677384551883,1.,1.13460291804635));
#27657=CARTESIAN_POINT('Ctrl Pts',(-1.76997111386806,-1.,1.14000548337));
#27658=CARTESIAN_POINT('Ctrl Pts',(-1.76997111386806,1.,1.14000548337));
#27659=CARTESIAN_POINT('Ctrl Pts',(-1.77313777896234,-1.,1.14543858226948));
#27660=CARTESIAN_POINT('Ctrl Pts',(-1.77313777896234,1.,1.14543858226948));
#27661=CARTESIAN_POINT('Ctrl Pts',(-1.77627422557034,-1.,1.15090197841531));
#27662=CARTESIAN_POINT('Ctrl Pts',(-1.77627422557034,1.,1.15090197841531));
#27663=CARTESIAN_POINT('Ctrl Pts',(-1.77938085564261,-1.,1.15639547194689));
#27664=CARTESIAN_POINT('Ctrl Pts',(-1.77938085564261,1.,1.15639547194689));
#27665=CARTESIAN_POINT('Ctrl Pts',(-1.78245795880949,-1.,1.16191881298458));
#27666=CARTESIAN_POINT('Ctrl Pts',(-1.78245795880949,1.,1.16191881298458));
#27667=CARTESIAN_POINT('Ctrl Pts',(-1.78550566040349,-1.,1.16747166312239));
#27668=CARTESIAN_POINT('Ctrl Pts',(-1.78550566040349,1.,1.16747166312239));
#27669=CARTESIAN_POINT('Ctrl Pts',(-1.78852398877523,-1.,1.17305363177265));
#27670=CARTESIAN_POINT('Ctrl Pts',(-1.78852398877523,1.,1.17305363177265));
#27671=CARTESIAN_POINT('Ctrl Pts',(-1.79151291552646,-1.,1.17866429440781));
#27672=CARTESIAN_POINT('Ctrl Pts',(-1.79151291552646,1.,1.17866429440781));
#27673=CARTESIAN_POINT('Ctrl Pts',(-1.79447240321572,-1.,1.18430321697471));
#27674=CARTESIAN_POINT('Ctrl Pts',(-1.79447240321572,1.,1.18430321697471));
#27675=CARTESIAN_POINT('Ctrl Pts',(-1.79740245923649,-1.,1.1899699793456));
#27676=CARTESIAN_POINT('Ctrl Pts',(-1.79740245923649,1.,1.1899699793456));
#27677=CARTESIAN_POINT('Ctrl Pts',(-1.80030314370121,-1.,1.19566418930405));
#27678=CARTESIAN_POINT('Ctrl Pts',(-1.80030314370121,1.,1.19566418930405));
#27679=CARTESIAN_POINT('Ctrl Pts',(-1.8031745483882,-1.,1.2013854893912));
#27680=CARTESIAN_POINT('Ctrl Pts',(-1.8031745483882,1.,1.2013854893912));
#27681=CARTESIAN_POINT('Ctrl Pts',(-1.80601678480772,-1.,1.20713356605519));
#27682=CARTESIAN_POINT('Ctrl Pts',(-1.80601678480772,1.,1.20713356605519));
#27683=CARTESIAN_POINT('Ctrl Pts',(-1.80882996916931,-1.,1.2129081570818));
#27684=CARTESIAN_POINT('Ctrl Pts',(-1.80882996916931,1.,1.2129081570818));
#27685=CARTESIAN_POINT('Ctrl Pts',(-1.81161420806172,-1.,1.2187090610323));
#27686=CARTESIAN_POINT('Ctrl Pts',(-1.81161420806172,1.,1.2187090610323));
#27687=CARTESIAN_POINT('Ctrl Pts',(-1.81436959209778,-1.,1.22453613304507));
#27688=CARTESIAN_POINT('Ctrl Pts',(-1.81436959209778,1.,1.22453613304507));
#27689=CARTESIAN_POINT('Ctrl Pts',(-1.81655087183054,-1.,1.22921864890975));
#27690=CARTESIAN_POINT('Ctrl Pts',(-1.81655087183054,1.,1.22921864890975));
#27691=CARTESIAN_POINT('Ctrl Pts',(-1.81817389920914,-1.,1.23274224526804));
#27692=CARTESIAN_POINT('Ctrl Pts',(-1.81817389920914,1.,1.23274224526804));
#27693=CARTESIAN_POINT('Ctrl Pts',(-1.81925017193531,-1.,1.23509651170384));
#27694=CARTESIAN_POINT('Ctrl Pts',(-1.81925017193531,1.,1.23509651170384));
#27695=CARTESIAN_POINT('Ctrl Pts',(-1.81978687191668,-1.,1.23627494547115));
#27696=CARTESIAN_POINT('Ctrl Pts',(-1.81978687191668,1.,1.23627494547115));
#27697=CARTESIAN_POINT('',(-1.5055822144029,1.,0.892032620296855));
#27698=CARTESIAN_POINT('Ctrl Pts',(-1.5055822144029,1.,0.892032620296855));
#27699=CARTESIAN_POINT('Ctrl Pts',(-1.50980486807181,1.,0.894452006967538));
#27700=CARTESIAN_POINT('Ctrl Pts',(-1.51805569591479,1.,0.89918504749193));
#27701=CARTESIAN_POINT('Ctrl Pts',(-1.52984849890434,1.,0.905967409640499));
#27702=CARTESIAN_POINT('Ctrl Pts',(-1.54440491152808,1.,0.91437591904658));
#27703=CARTESIAN_POINT('Ctrl Pts',(-1.56065988582509,1.,0.923832188966322));
#27704=CARTESIAN_POINT('Ctrl Pts',(-1.57499388385561,1.,0.932246680128849));
#27705=CARTESIAN_POINT('Ctrl Pts',(-1.58744937489796,1.,0.939646377909319));
#27706=CARTESIAN_POINT('Ctrl Pts',(-1.59810042045408,1.,0.946078063325796));
#27707=CARTESIAN_POINT('Ctrl Pts',(-1.60706069897794,1.,0.951613284361248));
#27708=CARTESIAN_POINT('Ctrl Pts',(-1.61449324337233,1.,0.956354422921573));
#27709=CARTESIAN_POINT('Ctrl Pts',(-1.62061638139929,1.,0.960438326099958));
#27710=CARTESIAN_POINT('Ctrl Pts',(-1.6257193066974,1.,0.964046107037821));
#27711=CARTESIAN_POINT('Ctrl Pts',(-1.63013849959083,1.,0.967387853228041));
#27712=CARTESIAN_POINT('Ctrl Pts',(-1.63420665729609,1.,0.970669715996356));
#27713=CARTESIAN_POINT('Ctrl Pts',(-1.63820952658157,1.,0.974066058287501));
#27714=CARTESIAN_POINT('Ctrl Pts',(-1.64233990826831,1.,0.977689794120297));
#27715=CARTESIAN_POINT('Ctrl Pts',(-1.64665139190834,1.,0.981562530940574));
#27716=CARTESIAN_POINT('Ctrl Pts',(-1.6511001661277,1.,0.985642622921626));
#27717=CARTESIAN_POINT('Ctrl Pts',(-1.65559044289746,1.,0.98985562785445));
#27718=CARTESIAN_POINT('Ctrl Pts',(-1.66001553809916,1.,0.994121836661116));
#27719=CARTESIAN_POINT('Ctrl Pts',(-1.66430758030304,1.,0.998389654952317));
#27720=CARTESIAN_POINT('Ctrl Pts',(-1.66846059277231,1.,1.00265091003682));
#27721=CARTESIAN_POINT('Ctrl Pts',(-1.67250335383248,1.,1.00692206696387));
#27722=CARTESIAN_POINT('Ctrl Pts',(-1.67648246776457,1.,1.01123236493507));
#27723=CARTESIAN_POINT('Ctrl Pts',(-1.6804428989482,1.,1.01561026162787));
#27724=CARTESIAN_POINT('Ctrl Pts',(-1.68440578021739,1.,1.02006795074222));
#27725=CARTESIAN_POINT('Ctrl Pts',(-1.68836910178475,1.,1.02460180535272));
#27726=CARTESIAN_POINT('Ctrl Pts',(-1.69231840863471,1.,1.02919977579155));
#27727=CARTESIAN_POINT('Ctrl Pts',(-1.69623414782769,1.,1.03384646003587));
#27728=CARTESIAN_POINT('Ctrl Pts',(-1.70010052930951,1.,1.03852922490782));
#27729=CARTESIAN_POINT('Ctrl Pts',(-1.70391338707969,1.,1.04324363334546));
#27730=CARTESIAN_POINT('Ctrl Pts',(-1.70767646263641,1.,1.0479908540499));
#27731=CARTESIAN_POINT('Ctrl Pts',(-1.71139783543986,1.,1.05277517202854));
#27732=CARTESIAN_POINT('Ctrl Pts',(-1.71508654427022,1.,1.05760163192481));
#27733=CARTESIAN_POINT('Ctrl Pts',(-1.71874858456908,1.,1.0624732468065));
#27734=CARTESIAN_POINT('Ctrl Pts',(-1.72238500928456,1.,1.06738966975463));
#27735=CARTESIAN_POINT('Ctrl Pts',(-1.72599406198489,1.,1.07234866990252));
#27736=CARTESIAN_POINT('Ctrl Pts',(-1.72957248977424,1.,1.0773470373727));
#27737=CARTESIAN_POINT('Ctrl Pts',(-1.73311705663407,1.,1.08238162784749));
#27738=CARTESIAN_POINT('Ctrl Pts',(-1.73662628326093,1.,1.08745056285429));
#27739=CARTESIAN_POINT('Ctrl Pts',(-1.74010053962252,1.,1.09255329056496));
#27740=CARTESIAN_POINT('Ctrl Pts',(-1.74354119236212,1.,1.09768999241229));
#27741=CARTESIAN_POINT('Ctrl Pts',(-1.74695004214924,1.,1.10286118991144));
#27742=CARTESIAN_POINT('Ctrl Pts',(-1.75032866075914,1.,1.10806728183003));
#27743=CARTESIAN_POINT('Ctrl Pts',(-1.75367772094617,1.,1.11330807582542));
#27744=CARTESIAN_POINT('Ctrl Pts',(-1.75699720772089,1.,1.11858293216752));
#27745=CARTESIAN_POINT('Ctrl Pts',(-1.76028671825084,1.,1.12389096855078));
#27746=CARTESIAN_POINT('Ctrl Pts',(-1.76354571966171,1.,1.12923123555076));
#27747=CARTESIAN_POINT('Ctrl Pts',(-1.76677384551883,1.,1.13460291804635));
#27748=CARTESIAN_POINT('Ctrl Pts',(-1.76997111386806,1.,1.14000548337));
#27749=CARTESIAN_POINT('Ctrl Pts',(-1.77313777896234,1.,1.14543858226948));
#27750=CARTESIAN_POINT('Ctrl Pts',(-1.77627422557034,1.,1.15090197841531));
#27751=CARTESIAN_POINT('Ctrl Pts',(-1.77938085564261,1.,1.15639547194689));
#27752=CARTESIAN_POINT('Ctrl Pts',(-1.78245795880949,1.,1.16191881298458));
#27753=CARTESIAN_POINT('Ctrl Pts',(-1.78550566040349,1.,1.16747166312239));
#27754=CARTESIAN_POINT('Ctrl Pts',(-1.78852398877523,1.,1.17305363177265));
#27755=CARTESIAN_POINT('Ctrl Pts',(-1.79151291552646,1.,1.17866429440781));
#27756=CARTESIAN_POINT('Ctrl Pts',(-1.79447240321572,1.,1.18430321697471));
#27757=CARTESIAN_POINT('Ctrl Pts',(-1.79740245923649,1.,1.1899699793456));
#27758=CARTESIAN_POINT('Ctrl Pts',(-1.80030314370121,1.,1.19566418930405));
#27759=CARTESIAN_POINT('Ctrl Pts',(-1.8031745483882,1.,1.2013854893912));
#27760=CARTESIAN_POINT('Ctrl Pts',(-1.80601678480772,1.,1.20713356605519));
#27761=CARTESIAN_POINT('Ctrl Pts',(-1.80882996916931,1.,1.2129081570818));
#27762=CARTESIAN_POINT('Ctrl Pts',(-1.81161420806172,1.,1.2187090610323));
#27763=CARTESIAN_POINT('Ctrl Pts',(-1.81436959209778,1.,1.22453613304507));
#27764=CARTESIAN_POINT('Ctrl Pts',(-1.81655087183054,1.,1.22921864890975));
#27765=CARTESIAN_POINT('Ctrl Pts',(-1.81817389920914,1.,1.23274224526804));
#27766=CARTESIAN_POINT('Ctrl Pts',(-1.81925017193531,1.,1.23509651170384));
#27767=CARTESIAN_POINT('Ctrl Pts',(-1.81978687191668,1.,1.23627494547115));
#27768=CARTESIAN_POINT('',(-1.5055822144029,0.,0.892032620296856));
#27769=CARTESIAN_POINT('Origin',(0.,0.,0.));
#27770=CARTESIAN_POINT('',(-1.60662857109684,1.,0.693717979106305));
#27771=CARTESIAN_POINT('Origin',(0.,1.,0.));
#27772=CARTESIAN_POINT('',(-1.60662857109684,0.,0.693717979106306));
#27773=CARTESIAN_POINT('Ctrl Pts',(-2.0698113262342,-1.,0.7455743247944));
#27774=CARTESIAN_POINT('Ctrl Pts',(-2.0698113262342,1.,0.7455743247944));
#27775=CARTESIAN_POINT('Ctrl Pts',(-2.06854248895728,-1.,0.745832791378367));
#27776=CARTESIAN_POINT('Ctrl Pts',(-2.06854248895728,1.,0.745832791378367));
#27777=CARTESIAN_POINT('Ctrl Pts',(-2.06600523016815,-1.,0.7463458715442));
#27778=CARTESIAN_POINT('Ctrl Pts',(-2.06600523016815,1.,0.7463458715442));
#27779=CARTESIAN_POINT('Ctrl Pts',(-2.06220058927826,-1.,0.747103932787919));
#27780=CARTESIAN_POINT('Ctrl Pts',(-2.06220058927826,1.,0.747103932787919));
#27781=CARTESIAN_POINT('Ctrl Pts',(-2.05713023031006,-1.,0.748091554183802));
#27782=CARTESIAN_POINT('Ctrl Pts',(-2.05713023031006,1.,0.748091554183802));
#27783=CARTESIAN_POINT('Ctrl Pts',(-2.05079645592154,-1.,0.749287468665046));
#27784=CARTESIAN_POINT('Ctrl Pts',(-2.05079645592154,1.,0.749287468665046));
#27785=CARTESIAN_POINT('Ctrl Pts',(-2.04446689147979,-1.,0.750444657875576));
#27786=CARTESIAN_POINT('Ctrl Pts',(-2.04446689147979,1.,0.750444657875576));
#27787=CARTESIAN_POINT('Ctrl Pts',(-2.03814160092099,-1.,0.751562963361115));
#27788=CARTESIAN_POINT('Ctrl Pts',(-2.03814160092099,1.,0.751562963361115));
#27789=CARTESIAN_POINT('Ctrl Pts',(-2.03182068456221,-1.,0.752642180487211));
#27790=CARTESIAN_POINT('Ctrl Pts',(-2.03182068456221,1.,0.752642180487211));
#27791=CARTESIAN_POINT('Ctrl Pts',(-2.02550428623313,-1.,0.753682061112768));
#27792=CARTESIAN_POINT('Ctrl Pts',(-2.02550428623313,1.,0.753682061112768));
#27793=CARTESIAN_POINT('Ctrl Pts',(-2.01919259405809,-1.,0.754682330722816));
#27794=CARTESIAN_POINT('Ctrl Pts',(-2.01919259405809,1.,0.754682330722816));
#27795=CARTESIAN_POINT('Ctrl Pts',(-2.01288584328084,-1.,0.755642704957865));
#27796=CARTESIAN_POINT('Ctrl Pts',(-2.01288584328084,1.,0.755642704957865));
#27797=CARTESIAN_POINT('Ctrl Pts',(-2.0065843158773,-1.,0.75656290464667));
#27798=CARTESIAN_POINT('Ctrl Pts',(-2.0065843158773,1.,0.75656290464667));
#27799=CARTESIAN_POINT('Ctrl Pts',(-2.00028834739178,-1.,0.757442676862724));
#27800=CARTESIAN_POINT('Ctrl Pts',(-2.00028834739178,1.,0.757442676862724));
#27801=CARTESIAN_POINT('Ctrl Pts',(-1.99399831098817,-1.,0.758281796766761));
#27802=CARTESIAN_POINT('Ctrl Pts',(-1.99399831098817,1.,0.758281796766761));
#27803=CARTESIAN_POINT('Ctrl Pts',(-1.98771456680874,-1.,0.759080037802488));
#27804=CARTESIAN_POINT('Ctrl Pts',(-1.98771456680874,1.,0.759080037802488));
#27805=CARTESIAN_POINT('Ctrl Pts',(-1.98143741418172,-1.,0.75983714745219));
#27806=CARTESIAN_POINT('Ctrl Pts',(-1.98143741418172,1.,0.75983714745219));
#27807=CARTESIAN_POINT('Ctrl Pts',(-1.97516705321494,-1.,0.760552825409757));
#27808=CARTESIAN_POINT('Ctrl Pts',(-1.97516705321494,1.,0.760552825409757));
#27809=CARTESIAN_POINT('Ctrl Pts',(-1.96890351582499,-1.,0.76122669048382));
#27810=CARTESIAN_POINT('Ctrl Pts',(-1.96890351582499,1.,0.76122669048382));
#27811=CARTESIAN_POINT('Ctrl Pts',(-1.96264672744186,-1.,0.761858300014423));
#27812=CARTESIAN_POINT('Ctrl Pts',(-1.96264672744186,1.,0.761858300014423));
#27813=CARTESIAN_POINT('Ctrl Pts',(-1.95639665309869,-1.,0.762447203806179));
#27814=CARTESIAN_POINT('Ctrl Pts',(-1.95639665309869,1.,0.762447203806179));
#27815=CARTESIAN_POINT('Ctrl Pts',(-1.95015342590024,-1.,0.762992990878769));
#27816=CARTESIAN_POINT('Ctrl Pts',(-1.95015342590024,1.,0.762992990878769));
#27817=CARTESIAN_POINT('Ctrl Pts',(-1.9439174661764,-1.,0.763495333538629));
#27818=CARTESIAN_POINT('Ctrl Pts',(-1.9439174661764,1.,0.763495333538629));
#27819=CARTESIAN_POINT('Ctrl Pts',(-1.93768964875886,-1.,0.763954049121458));
#27820=CARTESIAN_POINT('Ctrl Pts',(-1.93768964875886,1.,0.763954049121458));
#27821=CARTESIAN_POINT('Ctrl Pts',(-1.93147105496382,-1.,0.76436901067394));
#27822=CARTESIAN_POINT('Ctrl Pts',(-1.93147105496382,1.,0.76436901067394));
#27823=CARTESIAN_POINT('Ctrl Pts',(-1.92526263537048,-1.,0.764740025488211));
#27824=CARTESIAN_POINT('Ctrl Pts',(-1.92526263537048,1.,0.764740025488211));
#27825=CARTESIAN_POINT('Ctrl Pts',(-1.91906491634196,-1.,0.765066729667088));
#27826=CARTESIAN_POINT('Ctrl Pts',(-1.91906491634196,1.,0.765066729667088));
#27827=CARTESIAN_POINT('Ctrl Pts',(-1.91287765805169,-1.,0.765348465884722));
#27828=CARTESIAN_POINT('Ctrl Pts',(-1.91287765805169,1.,0.765348465884722));
#27829=CARTESIAN_POINT('Ctrl Pts',(-1.90669961402356,-1.,0.765584196937919));
#27830=CARTESIAN_POINT('Ctrl Pts',(-1.90669961402356,1.,0.765584196937919));
#27831=CARTESIAN_POINT('Ctrl Pts',(-1.90052930393596,-1.,0.765772772593386));
#27832=CARTESIAN_POINT('Ctrl Pts',(-1.90052930393596,1.,0.765772772593386));
#27833=CARTESIAN_POINT('Ctrl Pts',(-1.89436577771388,-1.,0.765913193856978));
#27834=CARTESIAN_POINT('Ctrl Pts',(-1.89436577771388,1.,0.765913193856978));
#27835=CARTESIAN_POINT('Ctrl Pts',(-1.88820926433409,-1.,0.766004837062091));
#27836=CARTESIAN_POINT('Ctrl Pts',(-1.88820926433409,1.,0.766004837062091));
#27837=CARTESIAN_POINT('Ctrl Pts',(-1.88206215302561,-1.,0.766047794851864));
#27838=CARTESIAN_POINT('Ctrl Pts',(-1.88206215302561,1.,0.766047794851864));
#27839=CARTESIAN_POINT('Ctrl Pts',(-1.87592888967883,-1.,0.766042837036744));
#27840=CARTESIAN_POINT('Ctrl Pts',(-1.87592888967883,1.,0.766042837036744));
#27841=CARTESIAN_POINT('Ctrl Pts',(-1.86981398314341,-1.,0.765990708546091));
#27842=CARTESIAN_POINT('Ctrl Pts',(-1.86981398314341,1.,0.765990708546091));
#27843=CARTESIAN_POINT('Ctrl Pts',(-1.86372027063312,-1.,0.765891519092547));
#27844=CARTESIAN_POINT('Ctrl Pts',(-1.86372027063312,1.,0.765891519092547));
#27845=CARTESIAN_POINT('Ctrl Pts',(-1.85764741390394,-1.,0.765744212909318));
#27846=CARTESIAN_POINT('Ctrl Pts',(-1.85764741390394,1.,0.765744212909318));
#27847=CARTESIAN_POINT('Ctrl Pts',(-1.85158945130063,-1.,0.765545710619062));
#27848=CARTESIAN_POINT('Ctrl Pts',(-1.85158945130063,1.,0.765545710619062));
#27849=CARTESIAN_POINT('Ctrl Pts',(-1.84553698875924,-1.,0.765291664862029));
#27850=CARTESIAN_POINT('Ctrl Pts',(-1.84553698875924,1.,0.765291664862029));
#27851=CARTESIAN_POINT('Ctrl Pts',(-1.83948181064835,-1.,0.764978057881737));
#27852=CARTESIAN_POINT('Ctrl Pts',(-1.83948181064835,1.,0.764978057881737));
#27853=CARTESIAN_POINT('Ctrl Pts',(-1.83342077227142,-1.,0.764602549687853));
#27854=CARTESIAN_POINT('Ctrl Pts',(-1.83342077227142,1.,0.764602549687853));
#27855=CARTESIAN_POINT('Ctrl Pts',(-1.82735991200065,-1.,0.764165902605995));
#27856=CARTESIAN_POINT('Ctrl Pts',(-1.82735991200065,1.,0.764165902605995));
#27857=CARTESIAN_POINT('Ctrl Pts',(-1.82131873145266,-1.,0.763673465462726));
#27858=CARTESIAN_POINT('Ctrl Pts',(-1.82131873145266,1.,0.763673465462726));
#27859=CARTESIAN_POINT('Ctrl Pts',(-1.8153211840553,-1.,0.763132003836634));
#27860=CARTESIAN_POINT('Ctrl Pts',(-1.8153211840553,1.,0.763132003836634));
#27861=CARTESIAN_POINT('Ctrl Pts',(-1.80938551463965,-1.,0.762546129463938));
#27862=CARTESIAN_POINT('Ctrl Pts',(-1.80938551463965,1.,0.762546129463938));
#27863=CARTESIAN_POINT('Ctrl Pts',(-1.80351583877342,-1.,0.761915336443547));
#27864=CARTESIAN_POINT('Ctrl Pts',(-1.80351583877342,1.,0.761915336443547));
#27865=CARTESIAN_POINT('Ctrl Pts',(-1.79768986997783,-1.,0.761229695230558));
#27866=CARTESIAN_POINT('Ctrl Pts',(-1.79768986997783,1.,0.761229695230558));
#27867=CARTESIAN_POINT('Ctrl Pts',(-1.7918581561088,-1.,0.760469555880749));
#27868=CARTESIAN_POINT('Ctrl Pts',(-1.7918581561088,1.,0.760469555880749));
#27869=CARTESIAN_POINT('Ctrl Pts',(-1.78596964884604,-1.,0.759614401110189));
#27870=CARTESIAN_POINT('Ctrl Pts',(-1.78596964884604,1.,0.759614401110189));
#27871=CARTESIAN_POINT('Ctrl Pts',(-1.77999411220945,-1.,0.758650626677518));
#27872=CARTESIAN_POINT('Ctrl Pts',(-1.77999411220945,1.,0.758650626677518));
#27873=CARTESIAN_POINT('Ctrl Pts',(-1.77394167108292,-1.,0.757578264077029));
#27874=CARTESIAN_POINT('Ctrl Pts',(-1.77394167108292,1.,0.757578264077029));
#27875=CARTESIAN_POINT('Ctrl Pts',(-1.76789396002998,-1.,0.75642189602781));
#27876=CARTESIAN_POINT('Ctrl Pts',(-1.76789396002998,1.,0.75642189602781));
#27877=CARTESIAN_POINT('Ctrl Pts',(-1.76197817240128,-1.,0.755220979974461));
#27878=CARTESIAN_POINT('Ctrl Pts',(-1.76197817240128,1.,0.755220979974461));
#27879=CARTESIAN_POINT('Ctrl Pts',(-1.75631083600019,-1.,0.754009254027829));
#27880=CARTESIAN_POINT('Ctrl Pts',(-1.75631083600019,1.,0.754009254027829));
#27881=CARTESIAN_POINT('Ctrl Pts',(-1.75095139468794,-1.,0.752797683531314));
#27882=CARTESIAN_POINT('Ctrl Pts',(-1.75095139468794,1.,0.752797683531314));
#27883=CARTESIAN_POINT('Ctrl Pts',(-1.74585086852502,-1.,0.751555614164482));
#27884=CARTESIAN_POINT('Ctrl Pts',(-1.74585086852502,1.,0.751555614164482));
#27885=CARTESIAN_POINT('Ctrl Pts',(-1.74080458267114,-1.,0.750193435981249));
#27886=CARTESIAN_POINT('Ctrl Pts',(-1.74080458267114,1.,0.750193435981249));
#27887=CARTESIAN_POINT('Ctrl Pts',(-1.7355035168033,-1.,0.74858246295687));
#27888=CARTESIAN_POINT('Ctrl Pts',(-1.7355035168033,1.,0.74858246295687));
#27889=CARTESIAN_POINT('Ctrl Pts',(-1.72958533647714,-1.,0.746574710097752));
#27890=CARTESIAN_POINT('Ctrl Pts',(-1.72958533647714,1.,0.746574710097752));
#27891=CARTESIAN_POINT('Ctrl Pts',(-1.72268229916769,-1.,0.744021445433093));
#27892=CARTESIAN_POINT('Ctrl Pts',(-1.72268229916769,1.,0.744021445433093));
#27893=CARTESIAN_POINT('Ctrl Pts',(-1.71447789751001,-1.,0.74079516202821));
#27894=CARTESIAN_POINT('Ctrl Pts',(-1.71447789751001,1.,0.74079516202821));
#27895=CARTESIAN_POINT('Ctrl Pts',(-1.70473309004249,-1.,0.736799665716932));
#27896=CARTESIAN_POINT('Ctrl Pts',(-1.70473309004249,1.,0.736799665716932));
#27897=CARTESIAN_POINT('Ctrl Pts',(-1.69326921972915,-1.,0.731963238685357));
#27898=CARTESIAN_POINT('Ctrl Pts',(-1.69326921972915,1.,0.731963238685357));
#27899=CARTESIAN_POINT('Ctrl Pts',(-1.67996158451922,-1.,0.726235967982445));
#27900=CARTESIAN_POINT('Ctrl Pts',(-1.67996158451922,1.,0.726235967982445));
#27901=CARTESIAN_POINT('Ctrl Pts',(-1.66472880551777,-1.,0.71958543378795));
#27902=CARTESIAN_POINT('Ctrl Pts',(-1.66472880551777,1.,0.71958543378795));
#27903=CARTESIAN_POINT('Ctrl Pts',(-1.64752408828442,-1.,0.711993139340447));
#27904=CARTESIAN_POINT('Ctrl Pts',(-1.64752408828442,1.,0.711993139340447));
#27905=CARTESIAN_POINT('Ctrl Pts',(-1.6321654166204,-1.,0.705159151977294));
#27906=CARTESIAN_POINT('Ctrl Pts',(-1.6321654166204,1.,0.705159151977294));
#27907=CARTESIAN_POINT('Ctrl Pts',(-1.61974673471117,-1.,0.699605146398837));
#27908=CARTESIAN_POINT('Ctrl Pts',(-1.61974673471117,1.,0.699605146398837));
#27909=CARTESIAN_POINT('Ctrl Pts',(-1.61106790957619,-1.,0.69571209787897));
#27910=CARTESIAN_POINT('Ctrl Pts',(-1.61106790957619,1.,0.69571209787897));
#27911=CARTESIAN_POINT('Ctrl Pts',(-1.60662857109684,-1.,0.693717979106305));
#27912=CARTESIAN_POINT('Ctrl Pts',(-1.60662857109684,1.,0.693717979106305));
#27913=CARTESIAN_POINT('',(-2.0698113262342,1.,0.7455743247944));
#27914=CARTESIAN_POINT('Ctrl Pts',(-2.0698113262342,1.,0.7455743247944));
#27915=CARTESIAN_POINT('Ctrl Pts',(-2.06854248895728,1.,0.745832791378367));
#27916=CARTESIAN_POINT('Ctrl Pts',(-2.06600523016815,1.,0.7463458715442));
#27917=CARTESIAN_POINT('Ctrl Pts',(-2.06220058927826,1.,0.747103932787919));
#27918=CARTESIAN_POINT('Ctrl Pts',(-2.05713023031006,1.,0.748091554183802));
#27919=CARTESIAN_POINT('Ctrl Pts',(-2.05079645592154,1.,0.749287468665046));
#27920=CARTESIAN_POINT('Ctrl Pts',(-2.04446689147979,1.,0.750444657875576));
#27921=CARTESIAN_POINT('Ctrl Pts',(-2.03814160092099,1.,0.751562963361115));
#27922=CARTESIAN_POINT('Ctrl Pts',(-2.03182068456221,1.,0.752642180487211));
#27923=CARTESIAN_POINT('Ctrl Pts',(-2.02550428623313,1.,0.753682061112768));
#27924=CARTESIAN_POINT('Ctrl Pts',(-2.01919259405809,1.,0.754682330722816));
#27925=CARTESIAN_POINT('Ctrl Pts',(-2.01288584328084,1.,0.755642704957865));
#27926=CARTESIAN_POINT('Ctrl Pts',(-2.0065843158773,1.,0.75656290464667));
#27927=CARTESIAN_POINT('Ctrl Pts',(-2.00028834739178,1.,0.757442676862724));
#27928=CARTESIAN_POINT('Ctrl Pts',(-1.99399831098817,1.,0.758281796766761));
#27929=CARTESIAN_POINT('Ctrl Pts',(-1.98771456680874,1.,0.759080037802488));
#27930=CARTESIAN_POINT('Ctrl Pts',(-1.98143741418172,1.,0.75983714745219));
#27931=CARTESIAN_POINT('Ctrl Pts',(-1.97516705321494,1.,0.760552825409757));
#27932=CARTESIAN_POINT('Ctrl Pts',(-1.96890351582499,1.,0.76122669048382));
#27933=CARTESIAN_POINT('Ctrl Pts',(-1.96264672744186,1.,0.761858300014423));
#27934=CARTESIAN_POINT('Ctrl Pts',(-1.95639665309869,1.,0.762447203806179));
#27935=CARTESIAN_POINT('Ctrl Pts',(-1.95015342590024,1.,0.762992990878769));
#27936=CARTESIAN_POINT('Ctrl Pts',(-1.9439174661764,1.,0.763495333538629));
#27937=CARTESIAN_POINT('Ctrl Pts',(-1.93768964875886,1.,0.763954049121458));
#27938=CARTESIAN_POINT('Ctrl Pts',(-1.93147105496382,1.,0.76436901067394));
#27939=CARTESIAN_POINT('Ctrl Pts',(-1.92526263537048,1.,0.764740025488211));
#27940=CARTESIAN_POINT('Ctrl Pts',(-1.91906491634196,1.,0.765066729667088));
#27941=CARTESIAN_POINT('Ctrl Pts',(-1.91287765805169,1.,0.765348465884722));
#27942=CARTESIAN_POINT('Ctrl Pts',(-1.90669961402356,1.,0.765584196937919));
#27943=CARTESIAN_POINT('Ctrl Pts',(-1.90052930393596,1.,0.765772772593386));
#27944=CARTESIAN_POINT('Ctrl Pts',(-1.89436577771388,1.,0.765913193856978));
#27945=CARTESIAN_POINT('Ctrl Pts',(-1.88820926433409,1.,0.766004837062091));
#27946=CARTESIAN_POINT('Ctrl Pts',(-1.88206215302561,1.,0.766047794851864));
#27947=CARTESIAN_POINT('Ctrl Pts',(-1.87592888967883,1.,0.766042837036744));
#27948=CARTESIAN_POINT('Ctrl Pts',(-1.86981398314341,1.,0.765990708546091));
#27949=CARTESIAN_POINT('Ctrl Pts',(-1.86372027063312,1.,0.765891519092547));
#27950=CARTESIAN_POINT('Ctrl Pts',(-1.85764741390394,1.,0.765744212909318));
#27951=CARTESIAN_POINT('Ctrl Pts',(-1.85158945130063,1.,0.765545710619062));
#27952=CARTESIAN_POINT('Ctrl Pts',(-1.84553698875924,1.,0.765291664862029));
#27953=CARTESIAN_POINT('Ctrl Pts',(-1.83948181064835,1.,0.764978057881737));
#27954=CARTESIAN_POINT('Ctrl Pts',(-1.83342077227142,1.,0.764602549687853));
#27955=CARTESIAN_POINT('Ctrl Pts',(-1.82735991200065,1.,0.764165902605995));
#27956=CARTESIAN_POINT('Ctrl Pts',(-1.82131873145266,1.,0.763673465462726));
#27957=CARTESIAN_POINT('Ctrl Pts',(-1.8153211840553,1.,0.763132003836634));
#27958=CARTESIAN_POINT('Ctrl Pts',(-1.80938551463965,1.,0.762546129463938));
#27959=CARTESIAN_POINT('Ctrl Pts',(-1.80351583877342,1.,0.761915336443547));
#27960=CARTESIAN_POINT('Ctrl Pts',(-1.79768986997783,1.,0.761229695230558));
#27961=CARTESIAN_POINT('Ctrl Pts',(-1.7918581561088,1.,0.760469555880749));
#27962=CARTESIAN_POINT('Ctrl Pts',(-1.78596964884604,1.,0.759614401110189));
#27963=CARTESIAN_POINT('Ctrl Pts',(-1.77999411220945,1.,0.758650626677518));
#27964=CARTESIAN_POINT('Ctrl Pts',(-1.77394167108292,1.,0.757578264077029));
#27965=CARTESIAN_POINT('Ctrl Pts',(-1.76789396002998,1.,0.75642189602781));
#27966=CARTESIAN_POINT('Ctrl Pts',(-1.76197817240128,1.,0.755220979974461));
#27967=CARTESIAN_POINT('Ctrl Pts',(-1.75631083600019,1.,0.754009254027829));
#27968=CARTESIAN_POINT('Ctrl Pts',(-1.75095139468794,1.,0.752797683531314));
#27969=CARTESIAN_POINT('Ctrl Pts',(-1.74585086852502,1.,0.751555614164482));
#27970=CARTESIAN_POINT('Ctrl Pts',(-1.74080458267114,1.,0.750193435981249));
#27971=CARTESIAN_POINT('Ctrl Pts',(-1.7355035168033,1.,0.74858246295687));
#27972=CARTESIAN_POINT('Ctrl Pts',(-1.72958533647714,1.,0.746574710097752));
#27973=CARTESIAN_POINT('Ctrl Pts',(-1.72268229916769,1.,0.744021445433093));
#27974=CARTESIAN_POINT('Ctrl Pts',(-1.71447789751001,1.,0.74079516202821));
#27975=CARTESIAN_POINT('Ctrl Pts',(-1.70473309004249,1.,0.736799665716932));
#27976=CARTESIAN_POINT('Ctrl Pts',(-1.69326921972915,1.,0.731963238685357));
#27977=CARTESIAN_POINT('Ctrl Pts',(-1.67996158451922,1.,0.726235967982445));
#27978=CARTESIAN_POINT('Ctrl Pts',(-1.66472880551777,1.,0.71958543378795));
#27979=CARTESIAN_POINT('Ctrl Pts',(-1.64752408828442,1.,0.711993139340447));
#27980=CARTESIAN_POINT('Ctrl Pts',(-1.6321654166204,1.,0.705159151977294));
#27981=CARTESIAN_POINT('Ctrl Pts',(-1.61974673471117,1.,0.699605146398837));
#27982=CARTESIAN_POINT('Ctrl Pts',(-1.61106790957619,1.,0.69571209787897));
#27983=CARTESIAN_POINT('Ctrl Pts',(-1.60662857109684,1.,0.693717979106305));
#27984=CARTESIAN_POINT('',(-2.0698113262342,0.,0.7455743247944));
#27985=CARTESIAN_POINT('Origin',(-2.11275013067528,0.,0.61342227326009));
#27986=CARTESIAN_POINT('',(-2.11275013067528,1.,0.61342227326009));
#27987=CARTESIAN_POINT('',(-2.0698113262342,1.,0.7455743247944));
#27988=CARTESIAN_POINT('',(-2.11275013067528,0.,0.61342227326009));
#27989=CARTESIAN_POINT('Ctrl Pts',(-1.7075470150345,-1.,0.383122945602004));
#27990=CARTESIAN_POINT('Ctrl Pts',(-1.7075470150345,1.,0.383122945602004));
#27991=CARTESIAN_POINT('Ctrl Pts',(-1.71231062891958,-1.,0.384119047315542));
#27992=CARTESIAN_POINT('Ctrl Pts',(-1.71231062891958,1.,0.384119047315542));
#27993=CARTESIAN_POINT('Ctrl Pts',(-1.72162022246158,-1.,0.38607079032701));
#27994=CARTESIAN_POINT('Ctrl Pts',(-1.72162022246158,1.,0.38607079032701));
#27995=CARTESIAN_POINT('Ctrl Pts',(-1.7349317097561,-1.,0.388877023509191));
#27996=CARTESIAN_POINT('Ctrl Pts',(-1.7349317097561,1.,0.388877023509191));
#27997=CARTESIAN_POINT('Ctrl Pts',(-1.75137405313962,-1.,0.392375812294307));
#27998=CARTESIAN_POINT('Ctrl Pts',(-1.75137405313962,1.,0.392375812294307));
#27999=CARTESIAN_POINT('Ctrl Pts',(-1.7697556004756,-1.,0.39634619612042));
#28000=CARTESIAN_POINT('Ctrl Pts',(-1.7697556004756,1.,0.39634619612042));
#28001=CARTESIAN_POINT('Ctrl Pts',(-1.78598826347533,-1.,0.39991940378308));
#28002=CARTESIAN_POINT('Ctrl Pts',(-1.78598826347533,1.,0.39991940378308));
#28003=CARTESIAN_POINT('Ctrl Pts',(-1.80012077176221,-1.,0.403107976170441));
#28004=CARTESIAN_POINT('Ctrl Pts',(-1.80012077176221,1.,0.403107976170441));
#28005=CARTESIAN_POINT('Ctrl Pts',(-1.81223801813988,-1.,0.405933518411838));
#28006=CARTESIAN_POINT('Ctrl Pts',(-1.81223801813988,1.,0.405933518411838));
#28007=CARTESIAN_POINT('Ctrl Pts',(-1.8224702267854,-1.,0.408428948108533));
#28008=CARTESIAN_POINT('Ctrl Pts',(-1.8224702267854,1.,0.408428948108533));
#28009=CARTESIAN_POINT('Ctrl Pts',(-1.83100408895216,-1.,0.410641256301675));
#28010=CARTESIAN_POINT('Ctrl Pts',(-1.83100408895216,1.,0.410641256301675));
#28011=CARTESIAN_POINT('Ctrl Pts',(-1.83808953475839,-1.,0.412633125322161));
#28012=CARTESIAN_POINT('Ctrl Pts',(-1.83808953475839,1.,0.412633125322161));
#28013=CARTESIAN_POINT('Ctrl Pts',(-1.8440575707371,-1.,0.41448743825434));
#28014=CARTESIAN_POINT('Ctrl Pts',(-1.8440575707371,1.,0.41448743825434));
#28015=CARTESIAN_POINT('Ctrl Pts',(-1.84929312929882,-1.,0.416300022038864));
#28016=CARTESIAN_POINT('Ctrl Pts',(-1.84929312929882,1.,0.416300022038864));
#28017=CARTESIAN_POINT('Ctrl Pts',(-1.85417632856234,-1.,0.418164129143534));
#28018=CARTESIAN_POINT('Ctrl Pts',(-1.85417632856234,1.,0.418164129143534));
#28019=CARTESIAN_POINT('Ctrl Pts',(-1.85903281096686,-1.,0.420157287975619));
#28020=CARTESIAN_POINT('Ctrl Pts',(-1.85903281096686,1.,0.420157287975619));
#28021=CARTESIAN_POINT('Ctrl Pts',(-1.86408083334028,-1.,0.422327307418275));
#28022=CARTESIAN_POINT('Ctrl Pts',(-1.86408083334028,1.,0.422327307418275));
#28023=CARTESIAN_POINT('Ctrl Pts',(-1.86937803944323,-1.,0.424678177291359));
#28024=CARTESIAN_POINT('Ctrl Pts',(-1.86937803944323,1.,0.424678177291359));
#28025=CARTESIAN_POINT('Ctrl Pts',(-1.87486989291484,-1.,0.427183828519102));
#28026=CARTESIAN_POINT('Ctrl Pts',(-1.87486989291484,1.,0.427183828519102));
#28027=CARTESIAN_POINT('Ctrl Pts',(-1.88044229001832,-1.,0.429803062482344));
#28028=CARTESIAN_POINT('Ctrl Pts',(-1.88044229001832,1.,0.429803062482344));
#28029=CARTESIAN_POINT('Ctrl Pts',(-1.88596913666793,-1.,0.432493038548748));
#28030=CARTESIAN_POINT('Ctrl Pts',(-1.88596913666793,1.,0.432493038548748));
#28031=CARTESIAN_POINT('Ctrl Pts',(-1.89136993975504,-1.,0.435225660963383));
#28032=CARTESIAN_POINT('Ctrl Pts',(-1.89136993975504,1.,0.435225660963383));
#28033=CARTESIAN_POINT('Ctrl Pts',(-1.89663648956466,-1.,0.437995003948244));
#28034=CARTESIAN_POINT('Ctrl Pts',(-1.89663648956466,1.,0.437995003948244));
#28035=CARTESIAN_POINT('Ctrl Pts',(-1.90180124389086,-1.,0.440807833704038));
#28036=CARTESIAN_POINT('Ctrl Pts',(-1.90180124389086,1.,0.440807833704038));
#28037=CARTESIAN_POINT('Ctrl Pts',(-1.90691756144898,-1.,0.44367755684915));
#28038=CARTESIAN_POINT('Ctrl Pts',(-1.90691756144898,1.,0.44367755684915));
#28039=CARTESIAN_POINT('Ctrl Pts',(-1.9120369998112,-1.,0.446617343485711));
#28040=CARTESIAN_POINT('Ctrl Pts',(-1.9120369998112,1.,0.446617343485711));
#28041=CARTESIAN_POINT('Ctrl Pts',(-1.91718342555755,-1.,0.449632260106662));
#28042=CARTESIAN_POINT('Ctrl Pts',(-1.91718342555755,1.,0.449632260106662));
#28043=CARTESIAN_POINT('Ctrl Pts',(-1.92235380648502,-1.,0.452719478359432));
#28044=CARTESIAN_POINT('Ctrl Pts',(-1.92235380648502,1.,0.452719478359432));
#28045=CARTESIAN_POINT('Ctrl Pts',(-1.92753067150476,-1.,0.455872005174371));
#28046=CARTESIAN_POINT('Ctrl Pts',(-1.92753067150476,1.,0.455872005174371));
#28047=CARTESIAN_POINT('Ctrl Pts',(-1.93269066517934,-1.,0.459081234547926));
#28048=CARTESIAN_POINT('Ctrl Pts',(-1.93269066517934,1.,0.459081234547926));
#28049=CARTESIAN_POINT('Ctrl Pts',(-1.93781486640821,-1.,0.462340031009056));
#28050=CARTESIAN_POINT('Ctrl Pts',(-1.93781486640821,1.,0.462340031009056));
#28051=CARTESIAN_POINT('Ctrl Pts',(-1.9428979419619,-1.,0.46564546202603));
#28052=CARTESIAN_POINT('Ctrl Pts',(-1.9428979419619,1.,0.46564546202603));
#28053=CARTESIAN_POINT('Ctrl Pts',(-1.94794381136514,-1.,0.468997482913135));
#28054=CARTESIAN_POINT('Ctrl Pts',(-1.94794381136514,1.,0.468997482913135));
#28055=CARTESIAN_POINT('Ctrl Pts',(-1.95296148278133,-1.,0.472397672264072));
#28056=CARTESIAN_POINT('Ctrl Pts',(-1.95296148278133,1.,0.472397672264072));
#28057=CARTESIAN_POINT('Ctrl Pts',(-1.95796111148177,-1.,0.475848034683176));
#28058=CARTESIAN_POINT('Ctrl Pts',(-1.95796111148177,1.,0.475848034683176));
#28059=CARTESIAN_POINT('Ctrl Pts',(-1.96294933055943,-1.,0.479349583074855));
#28060=CARTESIAN_POINT('Ctrl Pts',(-1.96294933055943,1.,0.479349583074855));
#28061=CARTESIAN_POINT('Ctrl Pts',(-1.96792703422362,-1.,0.48290166212069));
#28062=CARTESIAN_POINT('Ctrl Pts',(-1.96792703422362,1.,0.48290166212069));
#28063=CARTESIAN_POINT('Ctrl Pts',(-1.97289186263272,-1.,0.486502692907659));
#28064=CARTESIAN_POINT('Ctrl Pts',(-1.97289186263272,1.,0.486502692907659));
#28065=CARTESIAN_POINT('Ctrl Pts',(-1.97783973019229,-1.,0.490150627860952));
#28066=CARTESIAN_POINT('Ctrl Pts',(-1.97783973019229,1.,0.490150627860952));
#28067=CARTESIAN_POINT('Ctrl Pts',(-1.98276658761821,-1.,0.493843476541494));
#28068=CARTESIAN_POINT('Ctrl Pts',(-1.98276658761821,1.,0.493843476541494));
#28069=CARTESIAN_POINT('Ctrl Pts',(-1.98767044752932,-1.,0.497579909545574));
#28070=CARTESIAN_POINT('Ctrl Pts',(-1.98767044752932,1.,0.497579909545574));
#28071=CARTESIAN_POINT('Ctrl Pts',(-1.99255149126155,-1.,0.501359287727146));
#28072=CARTESIAN_POINT('Ctrl Pts',(-1.99255149126155,1.,0.501359287727146));
#28073=CARTESIAN_POINT('Ctrl Pts',(-1.99741107463572,-1.,0.505181361323026));
#28074=CARTESIAN_POINT('Ctrl Pts',(-1.99741107463572,1.,0.505181361323026));
#28075=CARTESIAN_POINT('Ctrl Pts',(-2.00225107134734,-1.,0.509046069886157));
#28076=CARTESIAN_POINT('Ctrl Pts',(-2.00225107134734,1.,0.509046069886157));
#28077=CARTESIAN_POINT('Ctrl Pts',(-2.00707309946949,-1.,0.512953306961792));
#28078=CARTESIAN_POINT('Ctrl Pts',(-2.00707309946949,1.,0.512953306961792));
#28079=CARTESIAN_POINT('Ctrl Pts',(-2.01187773939242,-1.,0.516902681728687));
#28080=CARTESIAN_POINT('Ctrl Pts',(-2.01187773939242,1.,0.516902681728687));
#28081=CARTESIAN_POINT('Ctrl Pts',(-2.01666477917286,-1.,0.52089359039937));
#28082=CARTESIAN_POINT('Ctrl Pts',(-2.01666477917286,1.,0.52089359039937));
#28083=CARTESIAN_POINT('Ctrl Pts',(-2.02143356304698,-1.,0.524925318333476));
#28084=CARTESIAN_POINT('Ctrl Pts',(-2.02143356304698,1.,0.524925318333476));
#28085=CARTESIAN_POINT('Ctrl Pts',(-2.0261832908329,-1.,0.528997127241914));
#28086=CARTESIAN_POINT('Ctrl Pts',(-2.0261832908329,1.,0.528997127241914));
#28087=CARTESIAN_POINT('Ctrl Pts',(-2.03091336214426,-1.,0.533108355132976));
#28088=CARTESIAN_POINT('Ctrl Pts',(-2.03091336214426,1.,0.533108355132976));
#28089=CARTESIAN_POINT('Ctrl Pts',(-2.03562362954037,-1.,0.537258489833262));
#28090=CARTESIAN_POINT('Ctrl Pts',(-2.03562362954037,1.,0.537258489833262));
#28091=CARTESIAN_POINT('Ctrl Pts',(-2.04031422690527,-1.,0.541447120615659));
#28092=CARTESIAN_POINT('Ctrl Pts',(-2.04031422690527,1.,0.541447120615659));
#28093=CARTESIAN_POINT('Ctrl Pts',(-2.04498544714588,-1.,0.54567390381743));
#28094=CARTESIAN_POINT('Ctrl Pts',(-2.04498544714588,1.,0.54567390381743));
#28095=CARTESIAN_POINT('Ctrl Pts',(-2.04963761077958,-1.,0.549938525150295));
#28096=CARTESIAN_POINT('Ctrl Pts',(-2.04963761077958,1.,0.549938525150295));
#28097=CARTESIAN_POINT('Ctrl Pts',(-2.05427091604413,-1.,0.554240657463906));
#28098=CARTESIAN_POINT('Ctrl Pts',(-2.05427091604413,1.,0.554240657463906));
#28099=CARTESIAN_POINT('Ctrl Pts',(-2.05888537756462,-1.,0.558579940185151));
#28100=CARTESIAN_POINT('Ctrl Pts',(-2.05888537756462,1.,0.558579940185151));
#28101=CARTESIAN_POINT('Ctrl Pts',(-2.06348090160589,-1.,0.562955993082261));
#28102=CARTESIAN_POINT('Ctrl Pts',(-2.06348090160589,1.,0.562955993082261));
#28103=CARTESIAN_POINT('Ctrl Pts',(-2.06805732997334,-1.,0.567368421181087));
#28104=CARTESIAN_POINT('Ctrl Pts',(-2.06805732997334,1.,0.567368421181087));
#28105=CARTESIAN_POINT('Ctrl Pts',(-2.07261449292824,-1.,0.571816823242603));
#28106=CARTESIAN_POINT('Ctrl Pts',(-2.07261449292824,1.,0.571816823242603));
#28107=CARTESIAN_POINT('Ctrl Pts',(-2.07715226767559,-1.,0.576300797416844));
#28108=CARTESIAN_POINT('Ctrl Pts',(-2.07715226767559,1.,0.576300797416844));
#28109=CARTESIAN_POINT('Ctrl Pts',(-2.08167059018418,-1.,0.580819952108063));
#28110=CARTESIAN_POINT('Ctrl Pts',(-2.08167059018418,1.,0.580819952108063));
#28111=CARTESIAN_POINT('Ctrl Pts',(-2.08616943727951,-1.,0.585373918991617));
#28112=CARTESIAN_POINT('Ctrl Pts',(-2.08616943727951,1.,0.585373918991617));
#28113=CARTESIAN_POINT('Ctrl Pts',(-2.09064881812129,-1.,0.589962365403406));
#28114=CARTESIAN_POINT('Ctrl Pts',(-2.09064881812129,1.,0.589962365403406));
#28115=CARTESIAN_POINT('Ctrl Pts',(-2.0951087622027,-1.,0.594585006052162));
#28116=CARTESIAN_POINT('Ctrl Pts',(-2.0951087622027,1.,0.594585006052162));
#28117=CARTESIAN_POINT('Ctrl Pts',(-2.0995493086477,-1.,0.599241616420533));
#28118=CARTESIAN_POINT('Ctrl Pts',(-2.0995493086477,1.,0.599241616420533));
#28119=CARTESIAN_POINT('Ctrl Pts',(-2.10397049886949,-1.,0.60393203073603));
#28120=CARTESIAN_POINT('Ctrl Pts',(-2.10397049886949,1.,0.60393203073603));
#28121=CARTESIAN_POINT('Ctrl Pts',(-2.1074919961518,-1.,0.607711315454876));
#28122=CARTESIAN_POINT('Ctrl Pts',(-2.1074919961518,1.,0.607711315454876));
#28123=CARTESIAN_POINT('Ctrl Pts',(-2.11012443807238,-1.,0.610560911689899));
#28124=CARTESIAN_POINT('Ctrl Pts',(-2.11012443807238,1.,0.610560911689899));
#28125=CARTESIAN_POINT('Ctrl Pts',(-2.11187554259986,-1.,0.6124673655618));
#28126=CARTESIAN_POINT('Ctrl Pts',(-2.11187554259986,1.,0.6124673655618));
#28127=CARTESIAN_POINT('Ctrl Pts',(-2.11275013067528,-1.,0.61342227326009));
#28128=CARTESIAN_POINT('Ctrl Pts',(-2.11275013067528,1.,0.61342227326009));
#28129=CARTESIAN_POINT('',(-1.7075470150345,1.,0.383122945602004));
#28130=CARTESIAN_POINT('Ctrl Pts',(-1.7075470150345,1.,0.383122945602004));
#28131=CARTESIAN_POINT('Ctrl Pts',(-1.71231062891958,1.,0.384119047315542));
#28132=CARTESIAN_POINT('Ctrl Pts',(-1.72162022246158,1.,0.38607079032701));
#28133=CARTESIAN_POINT('Ctrl Pts',(-1.7349317097561,1.,0.388877023509191));
#28134=CARTESIAN_POINT('Ctrl Pts',(-1.75137405313962,1.,0.392375812294307));
#28135=CARTESIAN_POINT('Ctrl Pts',(-1.7697556004756,1.,0.39634619612042));
#28136=CARTESIAN_POINT('Ctrl Pts',(-1.78598826347533,1.,0.39991940378308));
#28137=CARTESIAN_POINT('Ctrl Pts',(-1.80012077176221,1.,0.403107976170441));
#28138=CARTESIAN_POINT('Ctrl Pts',(-1.81223801813988,1.,0.405933518411838));
#28139=CARTESIAN_POINT('Ctrl Pts',(-1.8224702267854,1.,0.408428948108533));
#28140=CARTESIAN_POINT('Ctrl Pts',(-1.83100408895216,1.,0.410641256301675));
#28141=CARTESIAN_POINT('Ctrl Pts',(-1.83808953475839,1.,0.412633125322161));
#28142=CARTESIAN_POINT('Ctrl Pts',(-1.8440575707371,1.,0.41448743825434));
#28143=CARTESIAN_POINT('Ctrl Pts',(-1.84929312929882,1.,0.416300022038864));
#28144=CARTESIAN_POINT('Ctrl Pts',(-1.85417632856234,1.,0.418164129143534));
#28145=CARTESIAN_POINT('Ctrl Pts',(-1.85903281096686,1.,0.420157287975619));
#28146=CARTESIAN_POINT('Ctrl Pts',(-1.86408083334028,1.,0.422327307418275));
#28147=CARTESIAN_POINT('Ctrl Pts',(-1.86937803944323,1.,0.424678177291359));
#28148=CARTESIAN_POINT('Ctrl Pts',(-1.87486989291484,1.,0.427183828519102));
#28149=CARTESIAN_POINT('Ctrl Pts',(-1.88044229001832,1.,0.429803062482344));
#28150=CARTESIAN_POINT('Ctrl Pts',(-1.88596913666793,1.,0.432493038548748));
#28151=CARTESIAN_POINT('Ctrl Pts',(-1.89136993975504,1.,0.435225660963383));
#28152=CARTESIAN_POINT('Ctrl Pts',(-1.89663648956466,1.,0.437995003948244));
#28153=CARTESIAN_POINT('Ctrl Pts',(-1.90180124389086,1.,0.440807833704038));
#28154=CARTESIAN_POINT('Ctrl Pts',(-1.90691756144898,1.,0.44367755684915));
#28155=CARTESIAN_POINT('Ctrl Pts',(-1.9120369998112,1.,0.446617343485711));
#28156=CARTESIAN_POINT('Ctrl Pts',(-1.91718342555755,1.,0.449632260106662));
#28157=CARTESIAN_POINT('Ctrl Pts',(-1.92235380648502,1.,0.452719478359432));
#28158=CARTESIAN_POINT('Ctrl Pts',(-1.92753067150476,1.,0.455872005174371));
#28159=CARTESIAN_POINT('Ctrl Pts',(-1.93269066517934,1.,0.459081234547926));
#28160=CARTESIAN_POINT('Ctrl Pts',(-1.93781486640821,1.,0.462340031009056));
#28161=CARTESIAN_POINT('Ctrl Pts',(-1.9428979419619,1.,0.46564546202603));
#28162=CARTESIAN_POINT('Ctrl Pts',(-1.94794381136514,1.,0.468997482913135));
#28163=CARTESIAN_POINT('Ctrl Pts',(-1.95296148278133,1.,0.472397672264072));
#28164=CARTESIAN_POINT('Ctrl Pts',(-1.95796111148177,1.,0.475848034683176));
#28165=CARTESIAN_POINT('Ctrl Pts',(-1.96294933055943,1.,0.479349583074855));
#28166=CARTESIAN_POINT('Ctrl Pts',(-1.96792703422362,1.,0.48290166212069));
#28167=CARTESIAN_POINT('Ctrl Pts',(-1.97289186263272,1.,0.486502692907659));
#28168=CARTESIAN_POINT('Ctrl Pts',(-1.97783973019229,1.,0.490150627860952));
#28169=CARTESIAN_POINT('Ctrl Pts',(-1.98276658761821,1.,0.493843476541494));
#28170=CARTESIAN_POINT('Ctrl Pts',(-1.98767044752932,1.,0.497579909545574));
#28171=CARTESIAN_POINT('Ctrl Pts',(-1.99255149126155,1.,0.501359287727146));
#28172=CARTESIAN_POINT('Ctrl Pts',(-1.99741107463572,1.,0.505181361323026));
#28173=CARTESIAN_POINT('Ctrl Pts',(-2.00225107134734,1.,0.509046069886157));
#28174=CARTESIAN_POINT('Ctrl Pts',(-2.00707309946949,1.,0.512953306961792));
#28175=CARTESIAN_POINT('Ctrl Pts',(-2.01187773939242,1.,0.516902681728687));
#28176=CARTESIAN_POINT('Ctrl Pts',(-2.01666477917286,1.,0.52089359039937));
#28177=CARTESIAN_POINT('Ctrl Pts',(-2.02143356304698,1.,0.524925318333476));
#28178=CARTESIAN_POINT('Ctrl Pts',(-2.0261832908329,1.,0.528997127241914));
#28179=CARTESIAN_POINT('Ctrl Pts',(-2.03091336214426,1.,0.533108355132976));
#28180=CARTESIAN_POINT('Ctrl Pts',(-2.03562362954037,1.,0.537258489833262));
#28181=CARTESIAN_POINT('Ctrl Pts',(-2.04031422690527,1.,0.541447120615659));
#28182=CARTESIAN_POINT('Ctrl Pts',(-2.04498544714588,1.,0.54567390381743));
#28183=CARTESIAN_POINT('Ctrl Pts',(-2.04963761077958,1.,0.549938525150295));
#28184=CARTESIAN_POINT('Ctrl Pts',(-2.05427091604413,1.,0.554240657463906));
#28185=CARTESIAN_POINT('Ctrl Pts',(-2.05888537756462,1.,0.558579940185151));
#28186=CARTESIAN_POINT('Ctrl Pts',(-2.06348090160589,1.,0.562955993082261));
#28187=CARTESIAN_POINT('Ctrl Pts',(-2.06805732997334,1.,0.567368421181087));
#28188=CARTESIAN_POINT('Ctrl Pts',(-2.07261449292824,1.,0.571816823242603));
#28189=CARTESIAN_POINT('Ctrl Pts',(-2.07715226767559,1.,0.576300797416844));
#28190=CARTESIAN_POINT('Ctrl Pts',(-2.08167059018418,1.,0.580819952108063));
#28191=CARTESIAN_POINT('Ctrl Pts',(-2.08616943727951,1.,0.585373918991617));
#28192=CARTESIAN_POINT('Ctrl Pts',(-2.09064881812129,1.,0.589962365403406));
#28193=CARTESIAN_POINT('Ctrl Pts',(-2.0951087622027,1.,0.594585006052162));
#28194=CARTESIAN_POINT('Ctrl Pts',(-2.0995493086477,1.,0.599241616420533));
#28195=CARTESIAN_POINT('Ctrl Pts',(-2.10397049886949,1.,0.60393203073603));
#28196=CARTESIAN_POINT('Ctrl Pts',(-2.1074919961518,1.,0.607711315454876));
#28197=CARTESIAN_POINT('Ctrl Pts',(-2.11012443807238,1.,0.610560911689899));
#28198=CARTESIAN_POINT('Ctrl Pts',(-2.11187554259986,1.,0.6124673655618));
#28199=CARTESIAN_POINT('Ctrl Pts',(-2.11275013067528,1.,0.61342227326009));
#28200=CARTESIAN_POINT('',(-1.7075470150345,0.,0.383122945602003));
#28201=CARTESIAN_POINT('Origin',(0.,0.,0.));
#28202=CARTESIAN_POINT('',(-1.74236521665491,1.,0.163289472382896));
#28203=CARTESIAN_POINT('Origin',(0.,1.,0.));
#28204=CARTESIAN_POINT('',(-1.74236521665491,0.,0.163289472382896));
#28205=CARTESIAN_POINT('Ctrl Pts',(-2.19890268624765,-1.,0.069476445021958));
#28206=CARTESIAN_POINT('Ctrl Pts',(-2.19890268624765,1.,0.069476445021958));
#28207=CARTESIAN_POINT('Ctrl Pts',(-2.19777582085423,-1.,0.0701143536325489));
#28208=CARTESIAN_POINT('Ctrl Pts',(-2.19777582085423,1.,0.0701143536325489));
#28209=CARTESIAN_POINT('Ctrl Pts',(-2.19552129484002,-1.,0.0713863779526153));
#28210=CARTESIAN_POINT('Ctrl Pts',(-2.19552129484002,1.,0.0713863779526153));
#28211=CARTESIAN_POINT('Ctrl Pts',(-2.19213712013662,-1.,0.0732830357306724));
#28212=CARTESIAN_POINT('Ctrl Pts',(-2.19213712013662,1.,0.0732830357306724));
#28213=CARTESIAN_POINT('Ctrl Pts',(-2.1876201139953,-1.,0.0757891465836146));
#28214=CARTESIAN_POINT('Ctrl Pts',(-2.1876201139953,1.,0.0757891465836146));
#28215=CARTESIAN_POINT('Ctrl Pts',(-2.18196589448887,-1.,0.0788837727685241));
#28216=CARTESIAN_POINT('Ctrl Pts',(-2.18196589448887,1.,0.0788837727685241));
#28217=CARTESIAN_POINT('Ctrl Pts',(-2.176303712113,-1.,0.0819402680872764));
#28218=CARTESIAN_POINT('Ctrl Pts',(-2.176303712113,1.,0.0819402680872764));
#28219=CARTESIAN_POINT('Ctrl Pts',(-2.17063357870952,-1.,0.0849584620835371));
#28220=CARTESIAN_POINT('Ctrl Pts',(-2.17063357870952,1.,0.0849584620835371));
#28221=CARTESIAN_POINT('Ctrl Pts',(-2.16495552645014,-1.,0.0879381291386921));
#28222=CARTESIAN_POINT('Ctrl Pts',(-2.16495552645014,1.,0.0879381291386921));
#28223=CARTESIAN_POINT('Ctrl Pts',(-2.15926961544516,-1.,0.0908789888107264));
#28224=CARTESIAN_POINT('Ctrl Pts',(-2.15926961544516,1.,0.0908789888107264));
#28225=CARTESIAN_POINT('Ctrl Pts',(-2.1535759397817,-1.,0.0937807218867642));
#28226=CARTESIAN_POINT('Ctrl Pts',(-2.1535759397817,1.,0.0937807218867642));
#28227=CARTESIAN_POINT('Ctrl Pts',(-2.14787463531795,-1.,0.0966429852305457));
#28228=CARTESIAN_POINT('Ctrl Pts',(-2.14787463531795,1.,0.0966429852305457));
#28229=CARTESIAN_POINT('Ctrl Pts',(-2.14216588396025,-1.,0.0994654261990914));
#28230=CARTESIAN_POINT('Ctrl Pts',(-2.14216588396025,1.,0.0994654261990914));
#28231=CARTESIAN_POINT('Ctrl Pts',(-2.13644992667165,-1.,0.1022477005561));
#28232=CARTESIAN_POINT('Ctrl Pts',(-2.13644992667165,1.,0.1022477005561));
#28233=CARTESIAN_POINT('Ctrl Pts',(-2.13072704887293,-1.,0.104989479152739));
#28234=CARTESIAN_POINT('Ctrl Pts',(-2.13072704887293,1.,0.104989479152739));
#28235=CARTESIAN_POINT('Ctrl Pts',(-2.12499752307,-1.,0.10769043523109));
#28236=CARTESIAN_POINT('Ctrl Pts',(-2.12499752307,1.,0.10769043523109));
#28237=CARTESIAN_POINT('Ctrl Pts',(-2.11926155590865,-1.,0.110350236135025));
#28238=CARTESIAN_POINT('Ctrl Pts',(-2.11926155590865,1.,0.110350236135025));
#28239=CARTESIAN_POINT('Ctrl Pts',(-2.11351924490306,-1.,0.112968534419737));
#28240=CARTESIAN_POINT('Ctrl Pts',(-2.11351924490306,1.,0.112968534419737));
#28241=CARTESIAN_POINT('Ctrl Pts',(-2.10777050261309,-1.,0.115544957687926));
#28242=CARTESIAN_POINT('Ctrl Pts',(-2.10777050261309,1.,0.115544957687926));
#28243=CARTESIAN_POINT('Ctrl Pts',(-2.102015121329,-1.,0.118079107988355));
#28244=CARTESIAN_POINT('Ctrl Pts',(-2.102015121329,1.,0.118079107988355));
#28245=CARTESIAN_POINT('Ctrl Pts',(-2.0962529286773,-1.,0.120570567965122));
#28246=CARTESIAN_POINT('Ctrl Pts',(-2.0962529286773,1.,0.120570567965122));
#28247=CARTESIAN_POINT('Ctrl Pts',(-2.09048392424825,-1.,0.123018905621083));
#28248=CARTESIAN_POINT('Ctrl Pts',(-2.09048392424825,1.,0.123018905621083));
#28249=CARTESIAN_POINT('Ctrl Pts',(-2.08470840653643,-1.,0.125423679412061));
#28250=CARTESIAN_POINT('Ctrl Pts',(-2.08470840653643,1.,0.125423679412061));
#28251=CARTESIAN_POINT('Ctrl Pts',(-2.07892715110987,-1.,0.12778444527612));
#28252=CARTESIAN_POINT('Ctrl Pts',(-2.07892715110987,1.,0.12778444527612));
#28253=CARTESIAN_POINT('Ctrl Pts',(-2.07314114713063,-1.,0.130100748328403));
#28254=CARTESIAN_POINT('Ctrl Pts',(-2.07314114713063,1.,0.130100748328403));
#28255=CARTESIAN_POINT('Ctrl Pts',(-2.06735123910326,-1.,0.13237211154771));
#28256=CARTESIAN_POINT('Ctrl Pts',(-2.06735123910326,1.,0.13237211154771));
#28257=CARTESIAN_POINT('Ctrl Pts',(-2.06155781517842,-1.,0.134598026192106));
#28258=CARTESIAN_POINT('Ctrl Pts',(-2.06155781517842,1.,0.134598026192106));
#28259=CARTESIAN_POINT('Ctrl Pts',(-2.05576044414264,-1.,0.136777941218043));
#28260=CARTESIAN_POINT('Ctrl Pts',(-2.05576044414264,1.,0.136777941218043));
#28261=CARTESIAN_POINT('Ctrl Pts',(-2.04995762001328,-1.,0.138911255368966));
#28262=CARTESIAN_POINT('Ctrl Pts',(-2.04995762001328,1.,0.138911255368966));
#28263=CARTESIAN_POINT('Ctrl Pts',(-2.04414757947916,-1.,0.140997332152546));
#28264=CARTESIAN_POINT('Ctrl Pts',(-2.04414757947916,1.,0.140997332152546));
#28265=CARTESIAN_POINT('Ctrl Pts',(-2.03832911025912,-1.,0.143035515058209));
#28266=CARTESIAN_POINT('Ctrl Pts',(-2.03832911025912,1.,0.143035515058209));
#28267=CARTESIAN_POINT('Ctrl Pts',(-2.03250223739942,-1.,0.145025140186057));
#28268=CARTESIAN_POINT('Ctrl Pts',(-2.03250223739942,1.,0.145025140186057));
#28269=CARTESIAN_POINT('Ctrl Pts',(-2.02666926182017,-1.,0.146965557332583));
#28270=CARTESIAN_POINT('Ctrl Pts',(-2.02666926182017,1.,0.146965557332583));
#28271=CARTESIAN_POINT('Ctrl Pts',(-2.02083464969894,-1.,0.148856124775337));
#28272=CARTESIAN_POINT('Ctrl Pts',(-2.02083464969894,1.,0.148856124775337));
#28273=CARTESIAN_POINT('Ctrl Pts',(-2.01500291940238,-1.,0.150696157673078));
#28274=CARTESIAN_POINT('Ctrl Pts',(-2.01500291940238,1.,0.150696157673078));
#28275=CARTESIAN_POINT('Ctrl Pts',(-2.00917680318424,-1.,0.15248488362145));
#28276=CARTESIAN_POINT('Ctrl Pts',(-2.00917680318424,1.,0.15248488362145));
#28277=CARTESIAN_POINT('Ctrl Pts',(-2.00335565310543,-1.,0.154221403049722));
#28278=CARTESIAN_POINT('Ctrl Pts',(-2.00335565310543,1.,0.154221403049722));
#28279=CARTESIAN_POINT('Ctrl Pts',(-1.99753284771497,-1.,0.155904629548783));
#28280=CARTESIAN_POINT('Ctrl Pts',(-1.99753284771497,1.,0.155904629548783));
#28281=CARTESIAN_POINT('Ctrl Pts',(-1.99169810931908,-1.,0.157533331459227));
#28282=CARTESIAN_POINT('Ctrl Pts',(-1.99169810931908,1.,0.157533331459227));
#28283=CARTESIAN_POINT('Ctrl Pts',(-1.98584238283292,-1.,0.159106226437299));
#28284=CARTESIAN_POINT('Ctrl Pts',(-1.98584238283292,1.,0.159106226437299));
#28285=CARTESIAN_POINT('Ctrl Pts',(-1.97996195437559,-1.,0.160622060784611));
#28286=CARTESIAN_POINT('Ctrl Pts',(-1.97996195437559,1.,0.160622060784611));
#28287=CARTESIAN_POINT('Ctrl Pts',(-1.97406280235188,-1.,0.162079693556288));
#28288=CARTESIAN_POINT('Ctrl Pts',(-1.97406280235188,1.,0.162079693556288));
#28289=CARTESIAN_POINT('Ctrl Pts',(-1.96816512677967,-1.,0.163478185457734));
#28290=CARTESIAN_POINT('Ctrl Pts',(-1.96816512677967,1.,0.163478185457734));
#28291=CARTESIAN_POINT('Ctrl Pts',(-1.96229379940136,-1.,0.164816568920269));
#28292=CARTESIAN_POINT('Ctrl Pts',(-1.96229379940136,1.,0.164816568920269));
#28293=CARTESIAN_POINT('Ctrl Pts',(-1.9564675971873,-1.,0.166093592002812));
#28294=CARTESIAN_POINT('Ctrl Pts',(-1.9564675971873,1.,0.166093592002812));
#28295=CARTESIAN_POINT('Ctrl Pts',(-1.95069027794294,-1.,0.167307501784475));
#28296=CARTESIAN_POINT('Ctrl Pts',(-1.95069027794294,1.,0.167307501784475));
#28297=CARTESIAN_POINT('Ctrl Pts',(-1.94493757756931,-1.,0.168455741607556));
#28298=CARTESIAN_POINT('Ctrl Pts',(-1.94493757756931,1.,0.168455741607556));
#28299=CARTESIAN_POINT('Ctrl Pts',(-1.93915639211581,-1.,0.169534904817491));
#28300=CARTESIAN_POINT('Ctrl Pts',(-1.93915639211581,1.,0.169534904817491));
#28301=CARTESIAN_POINT('Ctrl Pts',(-1.93329183155539,-1.,0.170541253116201));
#28302=CARTESIAN_POINT('Ctrl Pts',(-1.93329183155539,1.,0.170541253116201));
#28303=CARTESIAN_POINT('Ctrl Pts',(-1.92731093582036,-1.,0.171471191532988));
#28304=CARTESIAN_POINT('Ctrl Pts',(-1.92731093582036,1.,0.171471191532988));
#28305=CARTESIAN_POINT('Ctrl Pts',(-1.9212233439798,-1.,0.172321621259514));
#28306=CARTESIAN_POINT('Ctrl Pts',(-1.9212233439798,1.,0.172321621259514));
#28307=CARTESIAN_POINT('Ctrl Pts',(-1.91511429159527,-1.,0.173090695383496));
#28308=CARTESIAN_POINT('Ctrl Pts',(-1.91511429159527,1.,0.173090695383496));
#28309=CARTESIAN_POINT('Ctrl Pts',(-1.90911693975267,-1.,0.173776635257817));
#28310=CARTESIAN_POINT('Ctrl Pts',(-1.90911693975267,1.,0.173776635257817));
#28311=CARTESIAN_POINT('Ctrl Pts',(-1.90335253862834,-1.,0.174375518661085));
#28312=CARTESIAN_POINT('Ctrl Pts',(-1.90335253862834,1.,0.174375518661085));
#28313=CARTESIAN_POINT('Ctrl Pts',(-1.89788101117132,-1.,0.174879405091263));
#28314=CARTESIAN_POINT('Ctrl Pts',(-1.89788101117132,1.,0.174879405091263));
#28315=CARTESIAN_POINT('Ctrl Pts',(-1.892646301985,-1.,0.175274276190844));
#28316=CARTESIAN_POINT('Ctrl Pts',(-1.892646301985,1.,0.175274276190844));
#28317=CARTESIAN_POINT('Ctrl Pts',(-1.88742606273259,-1.,0.175538155840648));
#28318=CARTESIAN_POINT('Ctrl Pts',(-1.88742606273259,1.,0.175538155840648));
#28319=CARTESIAN_POINT('Ctrl Pts',(-1.88188663145367,-1.,0.175644148889698));
#28320=CARTESIAN_POINT('Ctrl Pts',(-1.88188663145367,1.,0.175644148889698));
#28321=CARTESIAN_POINT('Ctrl Pts',(-1.87563767773588,-1.,0.175563480746485));
#28322=CARTESIAN_POINT('Ctrl Pts',(-1.87563767773588,1.,0.175563480746485));
#28323=CARTESIAN_POINT('Ctrl Pts',(-1.86828349694799,-1.,0.175268337590758));
#28324=CARTESIAN_POINT('Ctrl Pts',(-1.86828349694799,1.,0.175268337590758));
#28325=CARTESIAN_POINT('Ctrl Pts',(-1.85948367088837,-1.,0.17473525927603));
#28326=CARTESIAN_POINT('Ctrl Pts',(-1.85948367088837,1.,0.17473525927603));
#28327=CARTESIAN_POINT('Ctrl Pts',(-1.8489811319852,-1.,0.173946627587731));
#28328=CARTESIAN_POINT('Ctrl Pts',(-1.8489811319852,1.,0.173946627587731));
#28329=CARTESIAN_POINT('Ctrl Pts',(-1.83658380527692,-1.,0.1728894428919));
#28330=CARTESIAN_POINT('Ctrl Pts',(-1.83658380527692,1.,0.1728894428919));
#28331=CARTESIAN_POINT('Ctrl Pts',(-1.82215766811545,-1.,0.171554770204119));
#28332=CARTESIAN_POINT('Ctrl Pts',(-1.82215766811545,1.,0.171554770204119));
#28333=CARTESIAN_POINT('Ctrl Pts',(-1.80561530629706,-1.,0.169936923904608));
#28334=CARTESIAN_POINT('Ctrl Pts',(-1.80561530629706,1.,0.169936923904608));
#28335=CARTESIAN_POINT('Ctrl Pts',(-1.7869064998507,-1.,0.168032772805197));
#28336=CARTESIAN_POINT('Ctrl Pts',(-1.7869064998507,1.,0.168032772805197));
#28337=CARTESIAN_POINT('Ctrl Pts',(-1.77018771684844,-1.,0.1662793551464));
#28338=CARTESIAN_POINT('Ctrl Pts',(-1.77018771684844,1.,0.1662793551464));
#28339=CARTESIAN_POINT('Ctrl Pts',(-1.75666056638427,-1.,0.164834765707158));
#28340=CARTESIAN_POINT('Ctrl Pts',(-1.75666056638427,1.,0.164834765707158));
#28341=CARTESIAN_POINT('Ctrl Pts',(-1.7472034950333,-1.,0.163814161002002));
#28342=CARTESIAN_POINT('Ctrl Pts',(-1.7472034950333,1.,0.163814161002002));
#28343=CARTESIAN_POINT('Ctrl Pts',(-1.74236521665491,-1.,0.163289472382896));
#28344=CARTESIAN_POINT('Ctrl Pts',(-1.74236521665491,1.,0.163289472382896));
#28345=CARTESIAN_POINT('',(-2.19890268624765,1.,0.069476445021958));
#28346=CARTESIAN_POINT('Ctrl Pts',(-2.19890268624765,1.,0.069476445021958));
#28347=CARTESIAN_POINT('Ctrl Pts',(-2.19777582085423,1.,0.0701143536325489));
#28348=CARTESIAN_POINT('Ctrl Pts',(-2.19552129484002,1.,0.0713863779526153));
#28349=CARTESIAN_POINT('Ctrl Pts',(-2.19213712013662,1.,0.0732830357306724));
#28350=CARTESIAN_POINT('Ctrl Pts',(-2.1876201139953,1.,0.0757891465836146));
#28351=CARTESIAN_POINT('Ctrl Pts',(-2.18196589448887,1.,0.0788837727685241));
#28352=CARTESIAN_POINT('Ctrl Pts',(-2.176303712113,1.,0.0819402680872764));
#28353=CARTESIAN_POINT('Ctrl Pts',(-2.17063357870952,1.,0.0849584620835371));
#28354=CARTESIAN_POINT('Ctrl Pts',(-2.16495552645014,1.,0.0879381291386921));
#28355=CARTESIAN_POINT('Ctrl Pts',(-2.15926961544516,1.,0.0908789888107264));
#28356=CARTESIAN_POINT('Ctrl Pts',(-2.1535759397817,1.,0.0937807218867642));
#28357=CARTESIAN_POINT('Ctrl Pts',(-2.14787463531795,1.,0.0966429852305457));
#28358=CARTESIAN_POINT('Ctrl Pts',(-2.14216588396025,1.,0.0994654261990914));
#28359=CARTESIAN_POINT('Ctrl Pts',(-2.13644992667165,1.,0.1022477005561));
#28360=CARTESIAN_POINT('Ctrl Pts',(-2.13072704887293,1.,0.104989479152739));
#28361=CARTESIAN_POINT('Ctrl Pts',(-2.12499752307,1.,0.10769043523109));
#28362=CARTESIAN_POINT('Ctrl Pts',(-2.11926155590865,1.,0.110350236135025));
#28363=CARTESIAN_POINT('Ctrl Pts',(-2.11351924490306,1.,0.112968534419737));
#28364=CARTESIAN_POINT('Ctrl Pts',(-2.10777050261309,1.,0.115544957687926));
#28365=CARTESIAN_POINT('Ctrl Pts',(-2.102015121329,1.,0.118079107988355));
#28366=CARTESIAN_POINT('Ctrl Pts',(-2.0962529286773,1.,0.120570567965122));
#28367=CARTESIAN_POINT('Ctrl Pts',(-2.09048392424825,1.,0.123018905621083));
#28368=CARTESIAN_POINT('Ctrl Pts',(-2.08470840653643,1.,0.125423679412061));
#28369=CARTESIAN_POINT('Ctrl Pts',(-2.07892715110987,1.,0.12778444527612));
#28370=CARTESIAN_POINT('Ctrl Pts',(-2.07314114713063,1.,0.130100748328403));
#28371=CARTESIAN_POINT('Ctrl Pts',(-2.06735123910326,1.,0.13237211154771));
#28372=CARTESIAN_POINT('Ctrl Pts',(-2.06155781517842,1.,0.134598026192106));
#28373=CARTESIAN_POINT('Ctrl Pts',(-2.05576044414264,1.,0.136777941218043));
#28374=CARTESIAN_POINT('Ctrl Pts',(-2.04995762001328,1.,0.138911255368966));
#28375=CARTESIAN_POINT('Ctrl Pts',(-2.04414757947916,1.,0.140997332152546));
#28376=CARTESIAN_POINT('Ctrl Pts',(-2.03832911025912,1.,0.143035515058209));
#28377=CARTESIAN_POINT('Ctrl Pts',(-2.03250223739942,1.,0.145025140186057));
#28378=CARTESIAN_POINT('Ctrl Pts',(-2.02666926182017,1.,0.146965557332583));
#28379=CARTESIAN_POINT('Ctrl Pts',(-2.02083464969894,1.,0.148856124775337));
#28380=CARTESIAN_POINT('Ctrl Pts',(-2.01500291940238,1.,0.150696157673078));
#28381=CARTESIAN_POINT('Ctrl Pts',(-2.00917680318424,1.,0.15248488362145));
#28382=CARTESIAN_POINT('Ctrl Pts',(-2.00335565310543,1.,0.154221403049722));
#28383=CARTESIAN_POINT('Ctrl Pts',(-1.99753284771497,1.,0.155904629548783));
#28384=CARTESIAN_POINT('Ctrl Pts',(-1.99169810931908,1.,0.157533331459227));
#28385=CARTESIAN_POINT('Ctrl Pts',(-1.98584238283292,1.,0.159106226437299));
#28386=CARTESIAN_POINT('Ctrl Pts',(-1.97996195437559,1.,0.160622060784611));
#28387=CARTESIAN_POINT('Ctrl Pts',(-1.97406280235188,1.,0.162079693556288));
#28388=CARTESIAN_POINT('Ctrl Pts',(-1.96816512677967,1.,0.163478185457734));
#28389=CARTESIAN_POINT('Ctrl Pts',(-1.96229379940136,1.,0.164816568920269));
#28390=CARTESIAN_POINT('Ctrl Pts',(-1.9564675971873,1.,0.166093592002812));
#28391=CARTESIAN_POINT('Ctrl Pts',(-1.95069027794294,1.,0.167307501784475));
#28392=CARTESIAN_POINT('Ctrl Pts',(-1.94493757756931,1.,0.168455741607556));
#28393=CARTESIAN_POINT('Ctrl Pts',(-1.93915639211581,1.,0.169534904817491));
#28394=CARTESIAN_POINT('Ctrl Pts',(-1.93329183155539,1.,0.170541253116201));
#28395=CARTESIAN_POINT('Ctrl Pts',(-1.92731093582036,1.,0.171471191532988));
#28396=CARTESIAN_POINT('Ctrl Pts',(-1.9212233439798,1.,0.172321621259514));
#28397=CARTESIAN_POINT('Ctrl Pts',(-1.91511429159527,1.,0.173090695383496));
#28398=CARTESIAN_POINT('Ctrl Pts',(-1.90911693975267,1.,0.173776635257817));
#28399=CARTESIAN_POINT('Ctrl Pts',(-1.90335253862834,1.,0.174375518661085));
#28400=CARTESIAN_POINT('Ctrl Pts',(-1.89788101117132,1.,0.174879405091263));
#28401=CARTESIAN_POINT('Ctrl Pts',(-1.892646301985,1.,0.175274276190844));
#28402=CARTESIAN_POINT('Ctrl Pts',(-1.88742606273259,1.,0.175538155840648));
#28403=CARTESIAN_POINT('Ctrl Pts',(-1.88188663145367,1.,0.175644148889698));
#28404=CARTESIAN_POINT('Ctrl Pts',(-1.87563767773588,1.,0.175563480746485));
#28405=CARTESIAN_POINT('Ctrl Pts',(-1.86828349694799,1.,0.175268337590758));
#28406=CARTESIAN_POINT('Ctrl Pts',(-1.85948367088837,1.,0.17473525927603));
#28407=CARTESIAN_POINT('Ctrl Pts',(-1.8489811319852,1.,0.173946627587731));
#28408=CARTESIAN_POINT('Ctrl Pts',(-1.83658380527692,1.,0.1728894428919));
#28409=CARTESIAN_POINT('Ctrl Pts',(-1.82215766811545,1.,0.171554770204119));
#28410=CARTESIAN_POINT('Ctrl Pts',(-1.80561530629706,1.,0.169936923904608));
#28411=CARTESIAN_POINT('Ctrl Pts',(-1.7869064998507,1.,0.168032772805197));
#28412=CARTESIAN_POINT('Ctrl Pts',(-1.77018771684844,1.,0.1662793551464));
#28413=CARTESIAN_POINT('Ctrl Pts',(-1.75666056638427,1.,0.164834765707158));
#28414=CARTESIAN_POINT('Ctrl Pts',(-1.7472034950333,1.,0.163814161002002));
#28415=CARTESIAN_POINT('Ctrl Pts',(-1.74236521665491,1.,0.163289472382896));
#28416=CARTESIAN_POINT('',(-2.19890268624765,0.,0.069476445021958));
#28417=CARTESIAN_POINT('Origin',(-2.19890268624765,0.,-0.0694764450219585));
#28418=CARTESIAN_POINT('',(-2.19890268624765,1.,-0.0694764450219585));
#28419=CARTESIAN_POINT('',(-2.19890268624765,1.,0.069476445021958));
#28420=CARTESIAN_POINT('',(-2.19890268624765,0.,-0.0694764450219585));
#28421=CARTESIAN_POINT('Ctrl Pts',(-1.74236521665491,-1.,-0.163289472382896));
#28422=CARTESIAN_POINT('Ctrl Pts',(-1.74236521665491,1.,-0.163289472382896));
#28423=CARTESIAN_POINT('Ctrl Pts',(-1.74720349503904,-1.,-0.163814161002474));
#28424=CARTESIAN_POINT('Ctrl Pts',(-1.74720349503904,1.,-0.163814161002474));
#28425=CARTESIAN_POINT('Ctrl Pts',(-1.75666056640041,-1.,-0.164834765708484));
#28426=CARTESIAN_POINT('Ctrl Pts',(-1.75666056640041,1.,-0.164834765708484));
#28427=CARTESIAN_POINT('Ctrl Pts',(-1.77018771687692,-1.,-0.166279355148738));
#28428=CARTESIAN_POINT('Ctrl Pts',(-1.77018771687692,1.,-0.166279355148738));
#28429=CARTESIAN_POINT('Ctrl Pts',(-1.78690649988931,-1.,-0.16803277280837));
#28430=CARTESIAN_POINT('Ctrl Pts',(-1.78690649988931,1.,-0.16803277280837));
#28431=CARTESIAN_POINT('Ctrl Pts',(-1.80561530633924,-1.,-0.169936923908078));
#28432=CARTESIAN_POINT('Ctrl Pts',(-1.80561530633924,1.,-0.169936923908078));
#28433=CARTESIAN_POINT('Ctrl Pts',(-1.82215766815414,-1.,-0.171554770207306));
#28434=CARTESIAN_POINT('Ctrl Pts',(-1.82215766815414,1.,-0.171554770207306));
#28435=CARTESIAN_POINT('Ctrl Pts',(-1.83658380530747,-1.,-0.17288944289442));
#28436=CARTESIAN_POINT('Ctrl Pts',(-1.83658380530747,1.,-0.17288944289442));
#28437=CARTESIAN_POINT('Ctrl Pts',(-1.84898113200543,-1.,-0.173946627589401));
#28438=CARTESIAN_POINT('Ctrl Pts',(-1.84898113200543,1.,-0.173946627589401));
#28439=CARTESIAN_POINT('Ctrl Pts',(-1.85948367089838,-1.,-0.174735259276856));
#28440=CARTESIAN_POINT('Ctrl Pts',(-1.85948367089838,1.,-0.174735259276856));
#28441=CARTESIAN_POINT('Ctrl Pts',(-1.86828349694972,-1.,-0.175268337590901));
#28442=CARTESIAN_POINT('Ctrl Pts',(-1.86828349694972,1.,-0.175268337590901));
#28443=CARTESIAN_POINT('Ctrl Pts',(-1.87563767773249,-1.,-0.175563480746205));
#28444=CARTESIAN_POINT('Ctrl Pts',(-1.87563767773249,1.,-0.175563480746205));
#28445=CARTESIAN_POINT('Ctrl Pts',(-1.88188663144846,-1.,-0.175644148889271));
#28446=CARTESIAN_POINT('Ctrl Pts',(-1.88188663144846,1.,-0.175644148889271));
#28447=CARTESIAN_POINT('Ctrl Pts',(-1.88742606272818,-1.,-0.175538155840286));
#28448=CARTESIAN_POINT('Ctrl Pts',(-1.88742606272818,1.,-0.175538155840286));
#28449=CARTESIAN_POINT('Ctrl Pts',(-1.89264630198279,-1.,-0.175274276190664));
#28450=CARTESIAN_POINT('Ctrl Pts',(-1.89264630198279,1.,-0.175274276190664));
#28451=CARTESIAN_POINT('Ctrl Pts',(-1.89788101117148,-1.,-0.174879405091277));
#28452=CARTESIAN_POINT('Ctrl Pts',(-1.89788101117148,1.,-0.174879405091277));
#28453=CARTESIAN_POINT('Ctrl Pts',(-1.90335253863003,-1.,-0.174375518661222));
#28454=CARTESIAN_POINT('Ctrl Pts',(-1.90335253863003,1.,-0.174375518661222));
#28455=CARTESIAN_POINT('Ctrl Pts',(-1.90911693975475,-1.,-0.173776635257984));
#28456=CARTESIAN_POINT('Ctrl Pts',(-1.90911693975475,1.,-0.173776635257984));
#28457=CARTESIAN_POINT('Ctrl Pts',(-1.91511429159681,-1.,-0.173090695383619));
#28458=CARTESIAN_POINT('Ctrl Pts',(-1.91511429159681,1.,-0.173090695383619));
#28459=CARTESIAN_POINT('Ctrl Pts',(-1.92122334398034,-1.,-0.172321621259557));
#28460=CARTESIAN_POINT('Ctrl Pts',(-1.92122334398034,1.,-0.172321621259557));
#28461=CARTESIAN_POINT('Ctrl Pts',(-1.92731093582,-1.,-0.17147119153296));
#28462=CARTESIAN_POINT('Ctrl Pts',(-1.92731093582,1.,-0.17147119153296));
#28463=CARTESIAN_POINT('Ctrl Pts',(-1.93329183155455,-1.,-0.170541253116136));
#28464=CARTESIAN_POINT('Ctrl Pts',(-1.93329183155455,1.,-0.170541253116136));
#28465=CARTESIAN_POINT('Ctrl Pts',(-1.93915639211497,-1.,-0.169534904817425));
#28466=CARTESIAN_POINT('Ctrl Pts',(-1.93915639211497,1.,-0.169534904817425));
#28467=CARTESIAN_POINT('Ctrl Pts',(-1.94493757756879,-1.,-0.168455741607516));
#28468=CARTESIAN_POINT('Ctrl Pts',(-1.94493757756879,1.,-0.168455741607516));
#28469=CARTESIAN_POINT('Ctrl Pts',(-1.95069027794286,-1.,-0.167307501784469));
#28470=CARTESIAN_POINT('Ctrl Pts',(-1.95069027794286,1.,-0.167307501784469));
#28471=CARTESIAN_POINT('Ctrl Pts',(-1.95646759718755,-1.,-0.166093592002833));
#28472=CARTESIAN_POINT('Ctrl Pts',(-1.95646759718755,1.,-0.166093592002833));
#28473=CARTESIAN_POINT('Ctrl Pts',(-1.96229379940174,-1.,-0.1648165689203));
#28474=CARTESIAN_POINT('Ctrl Pts',(-1.96229379940174,1.,-0.1648165689203));
#28475=CARTESIAN_POINT('Ctrl Pts',(-1.96816512678,-1.,-0.16347818545776));
#28476=CARTESIAN_POINT('Ctrl Pts',(-1.96816512678,1.,-0.16347818545776));
#28477=CARTESIAN_POINT('Ctrl Pts',(-1.97406280235204,-1.,-0.162079693556302));
#28478=CARTESIAN_POINT('Ctrl Pts',(-1.97406280235204,1.,-0.162079693556302));
#28479=CARTESIAN_POINT('Ctrl Pts',(-1.97996195437557,-1.,-0.16062206078461));
#28480=CARTESIAN_POINT('Ctrl Pts',(-1.97996195437557,1.,-0.16062206078461));
#28481=CARTESIAN_POINT('Ctrl Pts',(-1.98584238283279,-1.,-0.159106226437289));
#28482=CARTESIAN_POINT('Ctrl Pts',(-1.98584238283279,1.,-0.159106226437289));
#28483=CARTESIAN_POINT('Ctrl Pts',(-1.99169810931893,-1.,-0.157533331459215));
#28484=CARTESIAN_POINT('Ctrl Pts',(-1.99169810931893,1.,-0.157533331459215));
#28485=CARTESIAN_POINT('Ctrl Pts',(-1.99753284771487,-1.,-0.155904629548775));
#28486=CARTESIAN_POINT('Ctrl Pts',(-1.99753284771487,1.,-0.155904629548775));
#28487=CARTESIAN_POINT('Ctrl Pts',(-2.00335565310539,-1.,-0.154221403049719));
#28488=CARTESIAN_POINT('Ctrl Pts',(-2.00335565310539,1.,-0.154221403049719));
#28489=CARTESIAN_POINT('Ctrl Pts',(-2.00917680318426,-1.,-0.152484883621452));
#28490=CARTESIAN_POINT('Ctrl Pts',(-2.00917680318426,1.,-0.152484883621452));
#28491=CARTESIAN_POINT('Ctrl Pts',(-2.01500291940243,-1.,-0.150696157673084));
#28492=CARTESIAN_POINT('Ctrl Pts',(-2.01500291940243,1.,-0.150696157673084));
#28493=CARTESIAN_POINT('Ctrl Pts',(-2.02083464969897,-1.,-0.148856124775343));
#28494=CARTESIAN_POINT('Ctrl Pts',(-2.02083464969897,1.,-0.148856124775343));
#28495=CARTESIAN_POINT('Ctrl Pts',(-2.02666926182017,-1.,-0.146965557332586));
#28496=CARTESIAN_POINT('Ctrl Pts',(-2.02666926182017,1.,-0.146965557332586));
#28497=CARTESIAN_POINT('Ctrl Pts',(-2.03250223739941,-1.,-0.145025140186058));
#28498=CARTESIAN_POINT('Ctrl Pts',(-2.03250223739941,1.,-0.145025140186058));
#28499=CARTESIAN_POINT('Ctrl Pts',(-2.03832911025913,-1.,-0.143035515058208));
#28500=CARTESIAN_POINT('Ctrl Pts',(-2.03832911025913,1.,-0.143035515058208));
#28501=CARTESIAN_POINT('Ctrl Pts',(-2.04414757947919,-1.,-0.140997332152545));
#28502=CARTESIAN_POINT('Ctrl Pts',(-2.04414757947919,1.,-0.140997332152545));
#28503=CARTESIAN_POINT('Ctrl Pts',(-2.04995762001333,-1.,-0.138911255368966));
#28504=CARTESIAN_POINT('Ctrl Pts',(-2.04995762001333,1.,-0.138911255368966));
#28505=CARTESIAN_POINT('Ctrl Pts',(-2.0557604441427,-1.,-0.136777941218044));
#28506=CARTESIAN_POINT('Ctrl Pts',(-2.0557604441427,1.,-0.136777941218044));
#28507=CARTESIAN_POINT('Ctrl Pts',(-2.06155781517844,-1.,-0.134598026192107));
#28508=CARTESIAN_POINT('Ctrl Pts',(-2.06155781517844,1.,-0.134598026192107));
#28509=CARTESIAN_POINT('Ctrl Pts',(-2.06735123910319,-1.,-0.13237211154771));
#28510=CARTESIAN_POINT('Ctrl Pts',(-2.06735123910319,1.,-0.13237211154771));
#28511=CARTESIAN_POINT('Ctrl Pts',(-2.07314114713047,-1.,-0.130100748328401));
#28512=CARTESIAN_POINT('Ctrl Pts',(-2.07314114713047,1.,-0.130100748328401));
#28513=CARTESIAN_POINT('Ctrl Pts',(-2.07892715110967,-1.,-0.127784445276116));
#28514=CARTESIAN_POINT('Ctrl Pts',(-2.07892715110967,1.,-0.127784445276116));
#28515=CARTESIAN_POINT('Ctrl Pts',(-2.08470840653628,-1.,-0.125423679412058));
#28516=CARTESIAN_POINT('Ctrl Pts',(-2.08470840653628,1.,-0.125423679412058));
#28517=CARTESIAN_POINT('Ctrl Pts',(-2.09048392424826,-1.,-0.123018905621083));
#28518=CARTESIAN_POINT('Ctrl Pts',(-2.09048392424826,1.,-0.123018905621083));
#28519=CARTESIAN_POINT('Ctrl Pts',(-2.09625292867756,-1.,-0.120570567965129));
#28520=CARTESIAN_POINT('Ctrl Pts',(-2.09625292867756,1.,-0.120570567965129));
#28521=CARTESIAN_POINT('Ctrl Pts',(-2.10201512132945,-1.,-0.118079107988368));
#28522=CARTESIAN_POINT('Ctrl Pts',(-2.10201512132945,1.,-0.118079107988368));
#28523=CARTESIAN_POINT('Ctrl Pts',(-2.10777050261359,-1.,-0.11554495768794));
#28524=CARTESIAN_POINT('Ctrl Pts',(-2.10777050261359,1.,-0.11554495768794));
#28525=CARTESIAN_POINT('Ctrl Pts',(-2.11351924490335,-1.,-0.112968534419746));
#28526=CARTESIAN_POINT('Ctrl Pts',(-2.11351924490335,1.,-0.112968534419746));
#28527=CARTESIAN_POINT('Ctrl Pts',(-2.11926155590849,-1.,-0.11035023613502));
#28528=CARTESIAN_POINT('Ctrl Pts',(-2.11926155590849,1.,-0.11035023613502));
#28529=CARTESIAN_POINT('Ctrl Pts',(-2.12499752306927,-1.,-0.107690435231068));
#28530=CARTESIAN_POINT('Ctrl Pts',(-2.12499752306927,1.,-0.107690435231068));
#28531=CARTESIAN_POINT('Ctrl Pts',(-2.1307270488718,-1.,-0.104989479152703));
#28532=CARTESIAN_POINT('Ctrl Pts',(-2.1307270488718,1.,-0.104989479152703));
#28533=CARTESIAN_POINT('Ctrl Pts',(-2.13644992667052,-1.,-0.102247700556064));
#28534=CARTESIAN_POINT('Ctrl Pts',(-2.13644992667052,1.,-0.102247700556064));
#28535=CARTESIAN_POINT('Ctrl Pts',(-2.14216588395974,-1.,-0.0994654261990744));
#28536=CARTESIAN_POINT('Ctrl Pts',(-2.14216588395974,1.,-0.0994654261990744));
#28537=CARTESIAN_POINT('Ctrl Pts',(-2.14787463531864,-1.,-0.096642985230569));
#28538=CARTESIAN_POINT('Ctrl Pts',(-2.14787463531864,1.,-0.096642985230569));
#28539=CARTESIAN_POINT('Ctrl Pts',(-2.15357593978377,-1.,-0.0937807218868346));
#28540=CARTESIAN_POINT('Ctrl Pts',(-2.15357593978377,1.,-0.0937807218868346));
#28541=CARTESIAN_POINT('Ctrl Pts',(-2.15926961544808,-1.,-0.0908789888108267));
#28542=CARTESIAN_POINT('Ctrl Pts',(-2.15926961544808,1.,-0.0908789888108267));
#28543=CARTESIAN_POINT('Ctrl Pts',(-2.16495552645275,-1.,-0.0879381291387824));
#28544=CARTESIAN_POINT('Ctrl Pts',(-2.16495552645275,1.,-0.0879381291387824));
#28545=CARTESIAN_POINT('Ctrl Pts',(-2.17063357871031,-1.,-0.0849584620835644));
#28546=CARTESIAN_POINT('Ctrl Pts',(-2.17063357871031,1.,-0.0849584620835644));
#28547=CARTESIAN_POINT('Ctrl Pts',(-2.1763037121106,-1.,-0.0819402680871941));
#28548=CARTESIAN_POINT('Ctrl Pts',(-2.1763037121106,1.,-0.0819402680871941));
#28549=CARTESIAN_POINT('Ctrl Pts',(-2.18196589448304,-1.,-0.0788837727683229));
#28550=CARTESIAN_POINT('Ctrl Pts',(-2.18196589448304,1.,-0.0788837727683229));
#28551=CARTESIAN_POINT('Ctrl Pts',(-2.1876201139874,-1.,-0.0757891465833413));
#28552=CARTESIAN_POINT('Ctrl Pts',(-2.1876201139874,1.,-0.0757891465833413));
#28553=CARTESIAN_POINT('Ctrl Pts',(-2.19213712012956,-1.,-0.0732830357304277));
#28554=CARTESIAN_POINT('Ctrl Pts',(-2.19213712012956,1.,-0.0732830357304277));
#28555=CARTESIAN_POINT('Ctrl Pts',(-2.19552129483562,-1.,-0.0713863779524629));
#28556=CARTESIAN_POINT('Ctrl Pts',(-2.19552129483562,1.,-0.0713863779524629));
#28557=CARTESIAN_POINT('Ctrl Pts',(-2.19777582085261,-1.,-0.0701143536324927));
#28558=CARTESIAN_POINT('Ctrl Pts',(-2.19777582085261,1.,-0.0701143536324927));
#28559=CARTESIAN_POINT('Ctrl Pts',(-2.19890268624765,-1.,-0.0694764450219585));
#28560=CARTESIAN_POINT('Ctrl Pts',(-2.19890268624765,1.,-0.0694764450219585));
#28561=CARTESIAN_POINT('',(-1.74236521665491,1.,-0.163289472382896));
#28562=CARTESIAN_POINT('Ctrl Pts',(-1.74236521665491,1.,-0.163289472382896));
#28563=CARTESIAN_POINT('Ctrl Pts',(-1.74720349503904,1.,-0.163814161002474));
#28564=CARTESIAN_POINT('Ctrl Pts',(-1.75666056640041,1.,-0.164834765708484));
#28565=CARTESIAN_POINT('Ctrl Pts',(-1.77018771687692,1.,-0.166279355148738));
#28566=CARTESIAN_POINT('Ctrl Pts',(-1.78690649988931,1.,-0.16803277280837));
#28567=CARTESIAN_POINT('Ctrl Pts',(-1.80561530633924,1.,-0.169936923908078));
#28568=CARTESIAN_POINT('Ctrl Pts',(-1.82215766815414,1.,-0.171554770207306));
#28569=CARTESIAN_POINT('Ctrl Pts',(-1.83658380530747,1.,-0.17288944289442));
#28570=CARTESIAN_POINT('Ctrl Pts',(-1.84898113200543,1.,-0.173946627589401));
#28571=CARTESIAN_POINT('Ctrl Pts',(-1.85948367089838,1.,-0.174735259276856));
#28572=CARTESIAN_POINT('Ctrl Pts',(-1.86828349694972,1.,-0.175268337590901));
#28573=CARTESIAN_POINT('Ctrl Pts',(-1.87563767773249,1.,-0.175563480746205));
#28574=CARTESIAN_POINT('Ctrl Pts',(-1.88188663144846,1.,-0.175644148889271));
#28575=CARTESIAN_POINT('Ctrl Pts',(-1.88742606272818,1.,-0.175538155840286));
#28576=CARTESIAN_POINT('Ctrl Pts',(-1.89264630198279,1.,-0.175274276190664));
#28577=CARTESIAN_POINT('Ctrl Pts',(-1.89788101117148,1.,-0.174879405091277));
#28578=CARTESIAN_POINT('Ctrl Pts',(-1.90335253863003,1.,-0.174375518661222));
#28579=CARTESIAN_POINT('Ctrl Pts',(-1.90911693975475,1.,-0.173776635257984));
#28580=CARTESIAN_POINT('Ctrl Pts',(-1.91511429159681,1.,-0.173090695383619));
#28581=CARTESIAN_POINT('Ctrl Pts',(-1.92122334398034,1.,-0.172321621259557));
#28582=CARTESIAN_POINT('Ctrl Pts',(-1.92731093582,1.,-0.17147119153296));
#28583=CARTESIAN_POINT('Ctrl Pts',(-1.93329183155455,1.,-0.170541253116136));
#28584=CARTESIAN_POINT('Ctrl Pts',(-1.93915639211497,1.,-0.169534904817425));
#28585=CARTESIAN_POINT('Ctrl Pts',(-1.94493757756879,1.,-0.168455741607516));
#28586=CARTESIAN_POINT('Ctrl Pts',(-1.95069027794286,1.,-0.167307501784469));
#28587=CARTESIAN_POINT('Ctrl Pts',(-1.95646759718755,1.,-0.166093592002833));
#28588=CARTESIAN_POINT('Ctrl Pts',(-1.96229379940174,1.,-0.1648165689203));
#28589=CARTESIAN_POINT('Ctrl Pts',(-1.96816512678,1.,-0.16347818545776));
#28590=CARTESIAN_POINT('Ctrl Pts',(-1.97406280235204,1.,-0.162079693556302));
#28591=CARTESIAN_POINT('Ctrl Pts',(-1.97996195437557,1.,-0.16062206078461));
#28592=CARTESIAN_POINT('Ctrl Pts',(-1.98584238283279,1.,-0.159106226437289));
#28593=CARTESIAN_POINT('Ctrl Pts',(-1.99169810931893,1.,-0.157533331459215));
#28594=CARTESIAN_POINT('Ctrl Pts',(-1.99753284771487,1.,-0.155904629548775));
#28595=CARTESIAN_POINT('Ctrl Pts',(-2.00335565310539,1.,-0.154221403049719));
#28596=CARTESIAN_POINT('Ctrl Pts',(-2.00917680318426,1.,-0.152484883621452));
#28597=CARTESIAN_POINT('Ctrl Pts',(-2.01500291940243,1.,-0.150696157673084));
#28598=CARTESIAN_POINT('Ctrl Pts',(-2.02083464969897,1.,-0.148856124775343));
#28599=CARTESIAN_POINT('Ctrl Pts',(-2.02666926182017,1.,-0.146965557332586));
#28600=CARTESIAN_POINT('Ctrl Pts',(-2.03250223739941,1.,-0.145025140186058));
#28601=CARTESIAN_POINT('Ctrl Pts',(-2.03832911025913,1.,-0.143035515058208));
#28602=CARTESIAN_POINT('Ctrl Pts',(-2.04414757947919,1.,-0.140997332152545));
#28603=CARTESIAN_POINT('Ctrl Pts',(-2.04995762001333,1.,-0.138911255368966));
#28604=CARTESIAN_POINT('Ctrl Pts',(-2.0557604441427,1.,-0.136777941218044));
#28605=CARTESIAN_POINT('Ctrl Pts',(-2.06155781517844,1.,-0.134598026192107));
#28606=CARTESIAN_POINT('Ctrl Pts',(-2.06735123910319,1.,-0.13237211154771));
#28607=CARTESIAN_POINT('Ctrl Pts',(-2.07314114713047,1.,-0.130100748328401));
#28608=CARTESIAN_POINT('Ctrl Pts',(-2.07892715110967,1.,-0.127784445276116));
#28609=CARTESIAN_POINT('Ctrl Pts',(-2.08470840653628,1.,-0.125423679412058));
#28610=CARTESIAN_POINT('Ctrl Pts',(-2.09048392424826,1.,-0.123018905621083));
#28611=CARTESIAN_POINT('Ctrl Pts',(-2.09625292867756,1.,-0.120570567965129));
#28612=CARTESIAN_POINT('Ctrl Pts',(-2.10201512132945,1.,-0.118079107988368));
#28613=CARTESIAN_POINT('Ctrl Pts',(-2.10777050261359,1.,-0.11554495768794));
#28614=CARTESIAN_POINT('Ctrl Pts',(-2.11351924490335,1.,-0.112968534419746));
#28615=CARTESIAN_POINT('Ctrl Pts',(-2.11926155590849,1.,-0.11035023613502));
#28616=CARTESIAN_POINT('Ctrl Pts',(-2.12499752306927,1.,-0.107690435231068));
#28617=CARTESIAN_POINT('Ctrl Pts',(-2.1307270488718,1.,-0.104989479152703));
#28618=CARTESIAN_POINT('Ctrl Pts',(-2.13644992667052,1.,-0.102247700556064));
#28619=CARTESIAN_POINT('Ctrl Pts',(-2.14216588395974,1.,-0.0994654261990744));
#28620=CARTESIAN_POINT('Ctrl Pts',(-2.14787463531864,1.,-0.096642985230569));
#28621=CARTESIAN_POINT('Ctrl Pts',(-2.15357593978377,1.,-0.0937807218868346));
#28622=CARTESIAN_POINT('Ctrl Pts',(-2.15926961544808,1.,-0.0908789888108267));
#28623=CARTESIAN_POINT('Ctrl Pts',(-2.16495552645275,1.,-0.0879381291387824));
#28624=CARTESIAN_POINT('Ctrl Pts',(-2.17063357871031,1.,-0.0849584620835644));
#28625=CARTESIAN_POINT('Ctrl Pts',(-2.1763037121106,1.,-0.0819402680871941));
#28626=CARTESIAN_POINT('Ctrl Pts',(-2.18196589448304,1.,-0.0788837727683229));
#28627=CARTESIAN_POINT('Ctrl Pts',(-2.1876201139874,1.,-0.0757891465833413));
#28628=CARTESIAN_POINT('Ctrl Pts',(-2.19213712012956,1.,-0.0732830357304277));
#28629=CARTESIAN_POINT('Ctrl Pts',(-2.19552129483562,1.,-0.0713863779524629));
#28630=CARTESIAN_POINT('Ctrl Pts',(-2.19777582085261,1.,-0.0701143536324927));
#28631=CARTESIAN_POINT('Ctrl Pts',(-2.19890268624765,1.,-0.0694764450219585));
#28632=CARTESIAN_POINT('',(-1.74236521665491,0.,-0.163289472382896));
#28633=CARTESIAN_POINT('Origin',(0.,0.,0.));
#28634=CARTESIAN_POINT('',(-1.7075470150345,1.,-0.383122945602004));
#28635=CARTESIAN_POINT('Origin',(0.,1.,0.));
#28636=CARTESIAN_POINT('',(-1.7075470150345,0.,-0.383122945602004));
#28637=CARTESIAN_POINT('Ctrl Pts',(-2.11275013067528,-1.,-0.61342227326009));
#28638=CARTESIAN_POINT('Ctrl Pts',(-2.11275013067528,1.,-0.61342227326009));
#28639=CARTESIAN_POINT('Ctrl Pts',(-2.11187554260142,-1.,-0.61246736556225));
#28640=CARTESIAN_POINT('Ctrl Pts',(-2.11187554260142,1.,-0.61246736556225));
#28641=CARTESIAN_POINT('Ctrl Pts',(-2.11012443807661,-1.,-0.610560911691113));
#28642=CARTESIAN_POINT('Ctrl Pts',(-2.11012443807661,1.,-0.610560911691113));
#28643=CARTESIAN_POINT('Ctrl Pts',(-2.10749199615859,-1.,-0.607711315456826));
#28644=CARTESIAN_POINT('Ctrl Pts',(-2.10749199615859,1.,-0.607711315456826));
#28645=CARTESIAN_POINT('Ctrl Pts',(-2.10397049887709,-1.,-0.603932030738212));
#28646=CARTESIAN_POINT('Ctrl Pts',(-2.10397049887709,1.,-0.603932030738212));
#28647=CARTESIAN_POINT('Ctrl Pts',(-2.09954930865331,-1.,-0.599241616422144));
#28648=CARTESIAN_POINT('Ctrl Pts',(-2.09954930865331,1.,-0.599241616422144));
#28649=CARTESIAN_POINT('Ctrl Pts',(-2.09510876220501,-1.,-0.594585006052823));
#28650=CARTESIAN_POINT('Ctrl Pts',(-2.09510876220501,1.,-0.594585006052823));
#28651=CARTESIAN_POINT('Ctrl Pts',(-2.09064881812053,-1.,-0.589962365403189));
#28652=CARTESIAN_POINT('Ctrl Pts',(-2.09064881812053,1.,-0.589962365403189));
#28653=CARTESIAN_POINT('Ctrl Pts',(-2.086169437277,-1.,-0.585373918990895));
#28654=CARTESIAN_POINT('Ctrl Pts',(-2.086169437277,1.,-0.585373918990895));
#28655=CARTESIAN_POINT('Ctrl Pts',(-2.08167059018138,-1.,-0.580819952107257));
#28656=CARTESIAN_POINT('Ctrl Pts',(-2.08167059018138,1.,-0.580819952107257));
#28657=CARTESIAN_POINT('Ctrl Pts',(-2.07715226767361,-1.,-0.576300797416274));
#28658=CARTESIAN_POINT('Ctrl Pts',(-2.07715226767361,1.,-0.576300797416274));
#28659=CARTESIAN_POINT('Ctrl Pts',(-2.07261449292757,-1.,-0.571816823242411));
#28660=CARTESIAN_POINT('Ctrl Pts',(-2.07261449292757,1.,-0.571816823242411));
#28661=CARTESIAN_POINT('Ctrl Pts',(-2.06805732997383,-1.,-0.567368421181229));
#28662=CARTESIAN_POINT('Ctrl Pts',(-2.06805732997383,1.,-0.567368421181229));
#28663=CARTESIAN_POINT('Ctrl Pts',(-2.06348090160697,-1.,-0.562955993082574));
#28664=CARTESIAN_POINT('Ctrl Pts',(-2.06348090160697,1.,-0.562955993082574));
#28665=CARTESIAN_POINT('Ctrl Pts',(-2.05888537756571,-1.,-0.558579940185467));
#28666=CARTESIAN_POINT('Ctrl Pts',(-2.05888537756571,1.,-0.558579940185467));
#28667=CARTESIAN_POINT('Ctrl Pts',(-2.05427091604482,-1.,-0.554240657464109));
#28668=CARTESIAN_POINT('Ctrl Pts',(-2.05427091604482,1.,-0.554240657464109));
#28669=CARTESIAN_POINT('Ctrl Pts',(-2.04963761077974,-1.,-0.549938525150342));
#28670=CARTESIAN_POINT('Ctrl Pts',(-2.04963761077974,1.,-0.549938525150342));
#28671=CARTESIAN_POINT('Ctrl Pts',(-2.0449854471456,-1.,-0.545673903817348));
#28672=CARTESIAN_POINT('Ctrl Pts',(-2.0449854471456,1.,-0.545673903817348));
#28673=CARTESIAN_POINT('Ctrl Pts',(-2.0403142269048,-1.,-0.54144712061552));
#28674=CARTESIAN_POINT('Ctrl Pts',(-2.0403142269048,1.,-0.54144712061552));
#28675=CARTESIAN_POINT('Ctrl Pts',(-2.03562362953993,-1.,-0.537258489833134));
#28676=CARTESIAN_POINT('Ctrl Pts',(-2.03562362953993,1.,-0.537258489833134));
#28677=CARTESIAN_POINT('Ctrl Pts',(-2.03091336214401,-1.,-0.533108355132905));
#28678=CARTESIAN_POINT('Ctrl Pts',(-2.03091336214401,1.,-0.533108355132905));
#28679=CARTESIAN_POINT('Ctrl Pts',(-2.02618329083289,-1.,-0.52899712724191));
#28680=CARTESIAN_POINT('Ctrl Pts',(-2.02618329083289,1.,-0.52899712724191));
#28681=CARTESIAN_POINT('Ctrl Pts',(-2.02143356304712,-1.,-0.524925318333518));
#28682=CARTESIAN_POINT('Ctrl Pts',(-2.02143356304712,1.,-0.524925318333518));
#28683=CARTESIAN_POINT('Ctrl Pts',(-2.01666477917305,-1.,-0.520893590399428));
#28684=CARTESIAN_POINT('Ctrl Pts',(-2.01666477917305,1.,-0.520893590399428));
#28685=CARTESIAN_POINT('Ctrl Pts',(-2.01187773939257,-1.,-0.516902681728733));
#28686=CARTESIAN_POINT('Ctrl Pts',(-2.01187773939257,1.,-0.516902681728733));
#28687=CARTESIAN_POINT('Ctrl Pts',(-2.00707309946955,-1.,-0.512953306961813));
#28688=CARTESIAN_POINT('Ctrl Pts',(-2.00707309946955,1.,-0.512953306961813));
#28689=CARTESIAN_POINT('Ctrl Pts',(-2.00225107134733,-1.,-0.509046069886152));
#28690=CARTESIAN_POINT('Ctrl Pts',(-2.00225107134733,1.,-0.509046069886152));
#28691=CARTESIAN_POINT('Ctrl Pts',(-1.99741107463567,-1.,-0.505181361323011));
#28692=CARTESIAN_POINT('Ctrl Pts',(-1.99741107463567,1.,-0.505181361323011));
#28693=CARTESIAN_POINT('Ctrl Pts',(-1.9925514912615,-1.,-0.501359287727129));
#28694=CARTESIAN_POINT('Ctrl Pts',(-1.9925514912615,1.,-0.501359287727129));
#28695=CARTESIAN_POINT('Ctrl Pts',(-1.98767044752929,-1.,-0.497579909545564));
#28696=CARTESIAN_POINT('Ctrl Pts',(-1.98767044752929,1.,-0.497579909545564));
#28697=CARTESIAN_POINT('Ctrl Pts',(-1.9827665876182,-1.,-0.493843476541492));
#28698=CARTESIAN_POINT('Ctrl Pts',(-1.9827665876182,1.,-0.493843476541492));
#28699=CARTESIAN_POINT('Ctrl Pts',(-1.97783973019229,-1.,-0.490150627860955));
#28700=CARTESIAN_POINT('Ctrl Pts',(-1.97783973019229,1.,-0.490150627860955));
#28701=CARTESIAN_POINT('Ctrl Pts',(-1.97289186263272,-1.,-0.486502692907661));
#28702=CARTESIAN_POINT('Ctrl Pts',(-1.97289186263272,1.,-0.486502692907661));
#28703=CARTESIAN_POINT('Ctrl Pts',(-1.96792703422358,-1.,-0.482901662120686));
#28704=CARTESIAN_POINT('Ctrl Pts',(-1.96792703422358,1.,-0.482901662120686));
#28705=CARTESIAN_POINT('Ctrl Pts',(-1.96294933055938,-1.,-0.479349583074846));
#28706=CARTESIAN_POINT('Ctrl Pts',(-1.96294933055938,1.,-0.479349583074846));
#28707=CARTESIAN_POINT('Ctrl Pts',(-1.95796111148175,-1.,-0.475848034683171));
#28708=CARTESIAN_POINT('Ctrl Pts',(-1.95796111148175,1.,-0.475848034683171));
#28709=CARTESIAN_POINT('Ctrl Pts',(-1.95296148278136,-1.,-0.472397672264079));
#28710=CARTESIAN_POINT('Ctrl Pts',(-1.95296148278136,1.,-0.472397672264079));
#28711=CARTESIAN_POINT('Ctrl Pts',(-1.94794381136524,-1.,-0.468997482913158));
#28712=CARTESIAN_POINT('Ctrl Pts',(-1.94794381136524,1.,-0.468997482913158));
#28713=CARTESIAN_POINT('Ctrl Pts',(-1.94289794196205,-1.,-0.465645462026064));
#28714=CARTESIAN_POINT('Ctrl Pts',(-1.94289794196205,1.,-0.465645462026064));
#28715=CARTESIAN_POINT('Ctrl Pts',(-1.93781486640834,-1.,-0.462340031009087));
#28716=CARTESIAN_POINT('Ctrl Pts',(-1.93781486640834,1.,-0.462340031009087));
#28717=CARTESIAN_POINT('Ctrl Pts',(-1.93269066517936,-1.,-0.459081234547931));
#28718=CARTESIAN_POINT('Ctrl Pts',(-1.93269066517936,1.,-0.459081234547931));
#28719=CARTESIAN_POINT('Ctrl Pts',(-1.92753067150461,-1.,-0.455872005174335));
#28720=CARTESIAN_POINT('Ctrl Pts',(-1.92753067150461,1.,-0.455872005174335));
#28721=CARTESIAN_POINT('Ctrl Pts',(-1.9223538064847,-1.,-0.452719478359356));
#28722=CARTESIAN_POINT('Ctrl Pts',(-1.9223538064847,1.,-0.452719478359356));
#28723=CARTESIAN_POINT('Ctrl Pts',(-1.91718342555717,-1.,-0.449632260106572));
#28724=CARTESIAN_POINT('Ctrl Pts',(-1.91718342555717,1.,-0.449632260106572));
#28725=CARTESIAN_POINT('Ctrl Pts',(-1.91203699981095,-1.,-0.446617343485651));
#28726=CARTESIAN_POINT('Ctrl Pts',(-1.91203699981095,1.,-0.446617343485651));
#28727=CARTESIAN_POINT('Ctrl Pts',(-1.90691756144906,-1.,-0.44367755684917));
#28728=CARTESIAN_POINT('Ctrl Pts',(-1.90691756144906,1.,-0.44367755684917));
#28729=CARTESIAN_POINT('Ctrl Pts',(-1.90180124389137,-1.,-0.44080783370416));
#28730=CARTESIAN_POINT('Ctrl Pts',(-1.90180124389137,1.,-0.44080783370416));
#28731=CARTESIAN_POINT('Ctrl Pts',(-1.89663648956549,-1.,-0.437995003948443));
#28732=CARTESIAN_POINT('Ctrl Pts',(-1.89663648956549,1.,-0.437995003948443));
#28733=CARTESIAN_POINT('Ctrl Pts',(-1.89136993975585,-1.,-0.43522566096358));
#28734=CARTESIAN_POINT('Ctrl Pts',(-1.89136993975585,1.,-0.43522566096358));
#28735=CARTESIAN_POINT('Ctrl Pts',(-1.88596913666828,-1.,-0.432493038548833));
#28736=CARTESIAN_POINT('Ctrl Pts',(-1.88596913666828,1.,-0.432493038548833));
#28737=CARTESIAN_POINT('Ctrl Pts',(-1.88044229001778,-1.,-0.429803062482217));
#28738=CARTESIAN_POINT('Ctrl Pts',(-1.88044229001778,1.,-0.429803062482217));
#28739=CARTESIAN_POINT('Ctrl Pts',(-1.87486989291333,-1.,-0.427183828518743));
#28740=CARTESIAN_POINT('Ctrl Pts',(-1.87486989291333,1.,-0.427183828518743));
#28741=CARTESIAN_POINT('Ctrl Pts',(-1.8693780394412,-1.,-0.424678177290876));
#28742=CARTESIAN_POINT('Ctrl Pts',(-1.8693780394412,1.,-0.424678177290876));
#28743=CARTESIAN_POINT('Ctrl Pts',(-1.86408083333863,-1.,-0.422327307417884));
#28744=CARTESIAN_POINT('Ctrl Pts',(-1.86408083333863,1.,-0.422327307417884));
#28745=CARTESIAN_POINT('Ctrl Pts',(-1.8590328109667,-1.,-0.420157287975583));
#28746=CARTESIAN_POINT('Ctrl Pts',(-1.8590328109667,1.,-0.420157287975583));
#28747=CARTESIAN_POINT('Ctrl Pts',(-1.8541763285645,-1.,-0.418164129144045));
#28748=CARTESIAN_POINT('Ctrl Pts',(-1.8541763285645,1.,-0.418164129144045));
#28749=CARTESIAN_POINT('Ctrl Pts',(-1.84929312930314,-1.,-0.416300022039885));
#28750=CARTESIAN_POINT('Ctrl Pts',(-1.84929312930314,1.,-0.416300022039885));
#28751=CARTESIAN_POINT('Ctrl Pts',(-1.84405757074218,-1.,-0.414487438255542));
#28752=CARTESIAN_POINT('Ctrl Pts',(-1.84405757074218,1.,-0.414487438255542));
#28753=CARTESIAN_POINT('Ctrl Pts',(-1.8380895347617,-1.,-0.412633125322945));
#28754=CARTESIAN_POINT('Ctrl Pts',(-1.8380895347617,1.,-0.412633125322945));
#28755=CARTESIAN_POINT('Ctrl Pts',(-1.83100408895047,-1.,-0.410641256301276));
#28756=CARTESIAN_POINT('Ctrl Pts',(-1.83100408895047,1.,-0.410641256301276));
#28757=CARTESIAN_POINT('Ctrl Pts',(-1.82247022677562,-1.,-0.408428948106227));
#28758=CARTESIAN_POINT('Ctrl Pts',(-1.82247022677562,1.,-0.408428948106227));
#28759=CARTESIAN_POINT('Ctrl Pts',(-1.81223801812013,-1.,-0.405933518407175));
#28760=CARTESIAN_POINT('Ctrl Pts',(-1.81223801812013,1.,-0.405933518407175));
#28761=CARTESIAN_POINT('Ctrl Pts',(-1.80012077173238,-1.,-0.403107976163396));
#28762=CARTESIAN_POINT('Ctrl Pts',(-1.80012077173238,1.,-0.403107976163396));
#28763=CARTESIAN_POINT('Ctrl Pts',(-1.78598826343754,-1.,-0.399919403774155));
#28764=CARTESIAN_POINT('Ctrl Pts',(-1.78598826343754,1.,-0.399919403774155));
#28765=CARTESIAN_POINT('Ctrl Pts',(-1.76975560043442,-1.,-0.396346196110688));
#28766=CARTESIAN_POINT('Ctrl Pts',(-1.76975560043442,1.,-0.396346196110688));
#28767=CARTESIAN_POINT('Ctrl Pts',(-1.75137405310193,-1.,-0.392375812285395));
#28768=CARTESIAN_POINT('Ctrl Pts',(-1.75137405310193,1.,-0.392375812285395));
#28769=CARTESIAN_POINT('Ctrl Pts',(-1.73493170972829,-1.,-0.388877023502615));
#28770=CARTESIAN_POINT('Ctrl Pts',(-1.73493170972829,1.,-0.388877023502615));
#28771=CARTESIAN_POINT('Ctrl Pts',(-1.72162022244582,-1.,-0.386070790323281));
#28772=CARTESIAN_POINT('Ctrl Pts',(-1.72162022244582,1.,-0.386070790323281));
#28773=CARTESIAN_POINT('Ctrl Pts',(-1.71231062891398,-1.,-0.384119047314215));
#28774=CARTESIAN_POINT('Ctrl Pts',(-1.71231062891398,1.,-0.384119047314215));
#28775=CARTESIAN_POINT('Ctrl Pts',(-1.7075470150345,-1.,-0.383122945602004));
#28776=CARTESIAN_POINT('Ctrl Pts',(-1.7075470150345,1.,-0.383122945602004));
#28777=CARTESIAN_POINT('',(-2.11275013067528,1.,-0.61342227326009));
#28778=CARTESIAN_POINT('Ctrl Pts',(-2.11275013067528,1.,-0.61342227326009));
#28779=CARTESIAN_POINT('Ctrl Pts',(-2.11187554260142,1.,-0.61246736556225));
#28780=CARTESIAN_POINT('Ctrl Pts',(-2.11012443807661,1.,-0.610560911691113));
#28781=CARTESIAN_POINT('Ctrl Pts',(-2.10749199615859,1.,-0.607711315456826));
#28782=CARTESIAN_POINT('Ctrl Pts',(-2.10397049887709,1.,-0.603932030738212));
#28783=CARTESIAN_POINT('Ctrl Pts',(-2.09954930865331,1.,-0.599241616422144));
#28784=CARTESIAN_POINT('Ctrl Pts',(-2.09510876220501,1.,-0.594585006052823));
#28785=CARTESIAN_POINT('Ctrl Pts',(-2.09064881812053,1.,-0.589962365403189));
#28786=CARTESIAN_POINT('Ctrl Pts',(-2.086169437277,1.,-0.585373918990895));
#28787=CARTESIAN_POINT('Ctrl Pts',(-2.08167059018138,1.,-0.580819952107257));
#28788=CARTESIAN_POINT('Ctrl Pts',(-2.07715226767361,1.,-0.576300797416274));
#28789=CARTESIAN_POINT('Ctrl Pts',(-2.07261449292757,1.,-0.571816823242411));
#28790=CARTESIAN_POINT('Ctrl Pts',(-2.06805732997383,1.,-0.567368421181229));
#28791=CARTESIAN_POINT('Ctrl Pts',(-2.06348090160697,1.,-0.562955993082574));
#28792=CARTESIAN_POINT('Ctrl Pts',(-2.05888537756571,1.,-0.558579940185467));
#28793=CARTESIAN_POINT('Ctrl Pts',(-2.05427091604482,1.,-0.554240657464109));
#28794=CARTESIAN_POINT('Ctrl Pts',(-2.04963761077974,1.,-0.549938525150342));
#28795=CARTESIAN_POINT('Ctrl Pts',(-2.0449854471456,1.,-0.545673903817348));
#28796=CARTESIAN_POINT('Ctrl Pts',(-2.0403142269048,1.,-0.54144712061552));
#28797=CARTESIAN_POINT('Ctrl Pts',(-2.03562362953993,1.,-0.537258489833134));
#28798=CARTESIAN_POINT('Ctrl Pts',(-2.03091336214401,1.,-0.533108355132905));
#28799=CARTESIAN_POINT('Ctrl Pts',(-2.02618329083289,1.,-0.52899712724191));
#28800=CARTESIAN_POINT('Ctrl Pts',(-2.02143356304712,1.,-0.524925318333518));
#28801=CARTESIAN_POINT('Ctrl Pts',(-2.01666477917305,1.,-0.520893590399428));
#28802=CARTESIAN_POINT('Ctrl Pts',(-2.01187773939257,1.,-0.516902681728733));
#28803=CARTESIAN_POINT('Ctrl Pts',(-2.00707309946955,1.,-0.512953306961813));
#28804=CARTESIAN_POINT('Ctrl Pts',(-2.00225107134733,1.,-0.509046069886152));
#28805=CARTESIAN_POINT('Ctrl Pts',(-1.99741107463567,1.,-0.505181361323011));
#28806=CARTESIAN_POINT('Ctrl Pts',(-1.9925514912615,1.,-0.501359287727129));
#28807=CARTESIAN_POINT('Ctrl Pts',(-1.98767044752929,1.,-0.497579909545564));
#28808=CARTESIAN_POINT('Ctrl Pts',(-1.9827665876182,1.,-0.493843476541492));
#28809=CARTESIAN_POINT('Ctrl Pts',(-1.97783973019229,1.,-0.490150627860955));
#28810=CARTESIAN_POINT('Ctrl Pts',(-1.97289186263272,1.,-0.486502692907661));
#28811=CARTESIAN_POINT('Ctrl Pts',(-1.96792703422358,1.,-0.482901662120686));
#28812=CARTESIAN_POINT('Ctrl Pts',(-1.96294933055938,1.,-0.479349583074846));
#28813=CARTESIAN_POINT('Ctrl Pts',(-1.95796111148175,1.,-0.475848034683171));
#28814=CARTESIAN_POINT('Ctrl Pts',(-1.95296148278136,1.,-0.472397672264079));
#28815=CARTESIAN_POINT('Ctrl Pts',(-1.94794381136524,1.,-0.468997482913158));
#28816=CARTESIAN_POINT('Ctrl Pts',(-1.94289794196205,1.,-0.465645462026064));
#28817=CARTESIAN_POINT('Ctrl Pts',(-1.93781486640834,1.,-0.462340031009087));
#28818=CARTESIAN_POINT('Ctrl Pts',(-1.93269066517936,1.,-0.459081234547931));
#28819=CARTESIAN_POINT('Ctrl Pts',(-1.92753067150461,1.,-0.455872005174335));
#28820=CARTESIAN_POINT('Ctrl Pts',(-1.9223538064847,1.,-0.452719478359356));
#28821=CARTESIAN_POINT('Ctrl Pts',(-1.91718342555717,1.,-0.449632260106572));
#28822=CARTESIAN_POINT('Ctrl Pts',(-1.91203699981095,1.,-0.446617343485651));
#28823=CARTESIAN_POINT('Ctrl Pts',(-1.90691756144906,1.,-0.44367755684917));
#28824=CARTESIAN_POINT('Ctrl Pts',(-1.90180124389137,1.,-0.44080783370416));
#28825=CARTESIAN_POINT('Ctrl Pts',(-1.89663648956549,1.,-0.437995003948443));
#28826=CARTESIAN_POINT('Ctrl Pts',(-1.89136993975585,1.,-0.43522566096358));
#28827=CARTESIAN_POINT('Ctrl Pts',(-1.88596913666828,1.,-0.432493038548833));
#28828=CARTESIAN_POINT('Ctrl Pts',(-1.88044229001778,1.,-0.429803062482217));
#28829=CARTESIAN_POINT('Ctrl Pts',(-1.87486989291333,1.,-0.427183828518743));
#28830=CARTESIAN_POINT('Ctrl Pts',(-1.8693780394412,1.,-0.424678177290876));
#28831=CARTESIAN_POINT('Ctrl Pts',(-1.86408083333863,1.,-0.422327307417884));
#28832=CARTESIAN_POINT('Ctrl Pts',(-1.8590328109667,1.,-0.420157287975583));
#28833=CARTESIAN_POINT('Ctrl Pts',(-1.8541763285645,1.,-0.418164129144045));
#28834=CARTESIAN_POINT('Ctrl Pts',(-1.84929312930314,1.,-0.416300022039885));
#28835=CARTESIAN_POINT('Ctrl Pts',(-1.84405757074218,1.,-0.414487438255542));
#28836=CARTESIAN_POINT('Ctrl Pts',(-1.8380895347617,1.,-0.412633125322945));
#28837=CARTESIAN_POINT('Ctrl Pts',(-1.83100408895047,1.,-0.410641256301276));
#28838=CARTESIAN_POINT('Ctrl Pts',(-1.82247022677562,1.,-0.408428948106227));
#28839=CARTESIAN_POINT('Ctrl Pts',(-1.81223801812013,1.,-0.405933518407175));
#28840=CARTESIAN_POINT('Ctrl Pts',(-1.80012077173238,1.,-0.403107976163396));
#28841=CARTESIAN_POINT('Ctrl Pts',(-1.78598826343754,1.,-0.399919403774155));
#28842=CARTESIAN_POINT('Ctrl Pts',(-1.76975560043442,1.,-0.396346196110688));
#28843=CARTESIAN_POINT('Ctrl Pts',(-1.75137405310193,1.,-0.392375812285395));
#28844=CARTESIAN_POINT('Ctrl Pts',(-1.73493170972829,1.,-0.388877023502615));
#28845=CARTESIAN_POINT('Ctrl Pts',(-1.72162022244582,1.,-0.386070790323281));
#28846=CARTESIAN_POINT('Ctrl Pts',(-1.71231062891398,1.,-0.384119047314215));
#28847=CARTESIAN_POINT('Ctrl Pts',(-1.7075470150345,1.,-0.383122945602004));
#28848=CARTESIAN_POINT('',(-2.11275013067528,0.,-0.61342227326009));
#28849=CARTESIAN_POINT('Origin',(-2.0698113262342,0.,-0.745574324794401));
#28850=CARTESIAN_POINT('',(-2.0698113262342,1.,-0.745574324794401));
#28851=CARTESIAN_POINT('',(-2.11275013067528,1.,-0.61342227326009));
#28852=CARTESIAN_POINT('',(-2.0698113262342,0.,-0.745574324794401));
#28853=CARTESIAN_POINT('Ctrl Pts',(-1.60662857109684,-1.,-0.693717979106306));
#28854=CARTESIAN_POINT('Ctrl Pts',(-1.60662857109684,1.,-0.693717979106306));
#28855=CARTESIAN_POINT('Ctrl Pts',(-1.61106790958151,-1.,-0.695712097881194));
#28856=CARTESIAN_POINT('Ctrl Pts',(-1.61106790958151,1.,-0.695712097881194));
#28857=CARTESIAN_POINT('Ctrl Pts',(-1.61974673472612,-1.,-0.699605146405088));
#28858=CARTESIAN_POINT('Ctrl Pts',(-1.61974673472612,1.,-0.699605146405088));
#28859=CARTESIAN_POINT('Ctrl Pts',(-1.63216541664676,-1.,-0.705159151988319));
#28860=CARTESIAN_POINT('Ctrl Pts',(-1.63216541664676,1.,-0.705159151988319));
#28861=CARTESIAN_POINT('Ctrl Pts',(-1.64752408832016,-1.,-0.711993139355394));
#28862=CARTESIAN_POINT('Ctrl Pts',(-1.64752408832016,1.,-0.711993139355394));
#28863=CARTESIAN_POINT('Ctrl Pts',(-1.6647288055568,-1.,-0.719585433804282));
#28864=CARTESIAN_POINT('Ctrl Pts',(-1.6647288055568,1.,-0.719585433804282));
#28865=CARTESIAN_POINT('Ctrl Pts',(-1.67996158455503,-1.,-0.726235967997433));
#28866=CARTESIAN_POINT('Ctrl Pts',(-1.67996158455503,1.,-0.726235967997433));
#28867=CARTESIAN_POINT('Ctrl Pts',(-1.69326921975743,-1.,-0.731963238697195));
#28868=CARTESIAN_POINT('Ctrl Pts',(-1.69326921975743,1.,-0.731963238697195));
#28869=CARTESIAN_POINT('Ctrl Pts',(-1.70473309006121,-1.,-0.736799665724771));
#28870=CARTESIAN_POINT('Ctrl Pts',(-1.70473309006121,1.,-0.736799665724771));
#28871=CARTESIAN_POINT('Ctrl Pts',(-1.71447789751927,-1.,-0.740795162032087));
#28872=CARTESIAN_POINT('Ctrl Pts',(-1.71447789751927,1.,-0.740795162032087));
#28873=CARTESIAN_POINT('Ctrl Pts',(-1.7226822991693,-1.,-0.744021445433764));
#28874=CARTESIAN_POINT('Ctrl Pts',(-1.7226822991693,1.,-0.744021445433764));
#28875=CARTESIAN_POINT('Ctrl Pts',(-1.72958533647399,-1.,-0.746574710096436));
#28876=CARTESIAN_POINT('Ctrl Pts',(-1.72958533647399,1.,-0.746574710096436));
#28877=CARTESIAN_POINT('Ctrl Pts',(-1.73550351679848,-1.,-0.748582462954854));
#28878=CARTESIAN_POINT('Ctrl Pts',(-1.73550351679848,1.,-0.748582462954854));
#28879=CARTESIAN_POINT('Ctrl Pts',(-1.74080458266705,-1.,-0.75019343597954));
#28880=CARTESIAN_POINT('Ctrl Pts',(-1.74080458266705,1.,-0.75019343597954));
#28881=CARTESIAN_POINT('Ctrl Pts',(-1.74585086852298,-1.,-0.751555614163629));
#28882=CARTESIAN_POINT('Ctrl Pts',(-1.74585086852298,1.,-0.751555614163629));
#28883=CARTESIAN_POINT('Ctrl Pts',(-1.75095139468809,-1.,-0.752797683531377));
#28884=CARTESIAN_POINT('Ctrl Pts',(-1.75095139468809,1.,-0.752797683531377));
#28885=CARTESIAN_POINT('Ctrl Pts',(-1.75631083600175,-1.,-0.75400925402848));
#28886=CARTESIAN_POINT('Ctrl Pts',(-1.75631083600175,1.,-0.75400925402848));
#28887=CARTESIAN_POINT('Ctrl Pts',(-1.7619781724032,-1.,-0.755220979975262));
#28888=CARTESIAN_POINT('Ctrl Pts',(-1.7619781724032,1.,-0.755220979975262));
#28889=CARTESIAN_POINT('Ctrl Pts',(-1.76789396003141,-1.,-0.756421896028403));
#28890=CARTESIAN_POINT('Ctrl Pts',(-1.76789396003141,1.,-0.756421896028403));
#28891=CARTESIAN_POINT('Ctrl Pts',(-1.77394167108342,-1.,-0.757578264077238));
#28892=CARTESIAN_POINT('Ctrl Pts',(-1.77394167108342,1.,-0.757578264077238));
#28893=CARTESIAN_POINT('Ctrl Pts',(-1.77999411220912,-1.,-0.75865062667738));
#28894=CARTESIAN_POINT('Ctrl Pts',(-1.77999411220912,1.,-0.75865062667738));
#28895=CARTESIAN_POINT('Ctrl Pts',(-1.78596964884526,-1.,-0.759614401109868));
#28896=CARTESIAN_POINT('Ctrl Pts',(-1.78596964884526,1.,-0.759614401109868));
#28897=CARTESIAN_POINT('Ctrl Pts',(-1.79185815610802,-1.,-0.760469555880425));
#28898=CARTESIAN_POINT('Ctrl Pts',(-1.79185815610802,1.,-0.760469555880425));
#28899=CARTESIAN_POINT('Ctrl Pts',(-1.79768986997735,-1.,-0.761229695230359));
#28900=CARTESIAN_POINT('Ctrl Pts',(-1.79768986997735,1.,-0.761229695230359));
#28901=CARTESIAN_POINT('Ctrl Pts',(-1.80351583877334,-1.,-0.761915336443515));
#28902=CARTESIAN_POINT('Ctrl Pts',(-1.80351583877334,1.,-0.761915336443515));
#28903=CARTESIAN_POINT('Ctrl Pts',(-1.80938551463989,-1.,-0.762546129464036));
#28904=CARTESIAN_POINT('Ctrl Pts',(-1.80938551463989,1.,-0.762546129464036));
#28905=CARTESIAN_POINT('Ctrl Pts',(-1.81532118405566,-1.,-0.763132003836783));
#28906=CARTESIAN_POINT('Ctrl Pts',(-1.81532118405566,1.,-0.763132003836783));
#28907=CARTESIAN_POINT('Ctrl Pts',(-1.82131873145297,-1.,-0.763673465462854));
#28908=CARTESIAN_POINT('Ctrl Pts',(-1.82131873145297,1.,-0.763673465462854));
#28909=CARTESIAN_POINT('Ctrl Pts',(-1.8273599120008,-1.,-0.764165902606055));
#28910=CARTESIAN_POINT('Ctrl Pts',(-1.8273599120008,1.,-0.764165902606055));
#28911=CARTESIAN_POINT('Ctrl Pts',(-1.8334207722714,-1.,-0.764602549687845));
#28912=CARTESIAN_POINT('Ctrl Pts',(-1.8334207722714,1.,-0.764602549687845));
#28913=CARTESIAN_POINT('Ctrl Pts',(-1.83948181064823,-1.,-0.764978057881687));
#28914=CARTESIAN_POINT('Ctrl Pts',(-1.83948181064823,1.,-0.764978057881687));
#28915=CARTESIAN_POINT('Ctrl Pts',(-1.8455369887591,-1.,-0.765291664861971));
#28916=CARTESIAN_POINT('Ctrl Pts',(-1.8455369887591,1.,-0.765291664861971));
#28917=CARTESIAN_POINT('Ctrl Pts',(-1.85158945130054,-1.,-0.765545710619023));
#28918=CARTESIAN_POINT('Ctrl Pts',(-1.85158945130054,1.,-0.765545710619023));
#28919=CARTESIAN_POINT('Ctrl Pts',(-1.85764741390391,-1.,-0.765744212909305));
#28920=CARTESIAN_POINT('Ctrl Pts',(-1.85764741390391,1.,-0.765744212909305));
#28921=CARTESIAN_POINT('Ctrl Pts',(-1.86372027063314,-1.,-0.765891519092557));
#28922=CARTESIAN_POINT('Ctrl Pts',(-1.86372027063314,1.,-0.765891519092557));
#28923=CARTESIAN_POINT('Ctrl Pts',(-1.86981398314345,-1.,-0.765990708546111));
#28924=CARTESIAN_POINT('Ctrl Pts',(-1.86981398314345,1.,-0.765990708546111));
#28925=CARTESIAN_POINT('Ctrl Pts',(-1.87592888967886,-1.,-0.766042837036759));
#28926=CARTESIAN_POINT('Ctrl Pts',(-1.87592888967886,1.,-0.766042837036759));
#28927=CARTESIAN_POINT('Ctrl Pts',(-1.88206215302561,-1.,-0.766047794851868));
#28928=CARTESIAN_POINT('Ctrl Pts',(-1.88206215302561,1.,-0.766047794851868));
#28929=CARTESIAN_POINT('Ctrl Pts',(-1.88820926433409,-1.,-0.76600483706209));
#28930=CARTESIAN_POINT('Ctrl Pts',(-1.88820926433409,1.,-0.76600483706209));
#28931=CARTESIAN_POINT('Ctrl Pts',(-1.89436577771389,-1.,-0.765913193856979));
#28932=CARTESIAN_POINT('Ctrl Pts',(-1.89436577771389,1.,-0.765913193856979));
#28933=CARTESIAN_POINT('Ctrl Pts',(-1.90052930393599,-1.,-0.765772772593395));
#28934=CARTESIAN_POINT('Ctrl Pts',(-1.90052930393599,1.,-0.765772772593395));
#28935=CARTESIAN_POINT('Ctrl Pts',(-1.90669961402362,-1.,-0.765584196937936));
#28936=CARTESIAN_POINT('Ctrl Pts',(-1.90669961402362,1.,-0.765584196937936));
#28937=CARTESIAN_POINT('Ctrl Pts',(-1.91287765805174,-1.,-0.765348465884739));
#28938=CARTESIAN_POINT('Ctrl Pts',(-1.91287765805174,1.,-0.765348465884739));
#28939=CARTESIAN_POINT('Ctrl Pts',(-1.91906491634197,-1.,-0.765066729667095));
#28940=CARTESIAN_POINT('Ctrl Pts',(-1.91906491634197,1.,-0.765066729667095));
#28941=CARTESIAN_POINT('Ctrl Pts',(-1.92526263537041,-1.,-0.764740025488189));
#28942=CARTESIAN_POINT('Ctrl Pts',(-1.92526263537041,1.,-0.764740025488189));
#28943=CARTESIAN_POINT('Ctrl Pts',(-1.93147105496367,-1.,-0.764369010673889));
#28944=CARTESIAN_POINT('Ctrl Pts',(-1.93147105496367,1.,-0.764369010673889));
#28945=CARTESIAN_POINT('Ctrl Pts',(-1.93768964875867,-1.,-0.763954049121393));
#28946=CARTESIAN_POINT('Ctrl Pts',(-1.93768964875867,1.,-0.763954049121393));
#28947=CARTESIAN_POINT('Ctrl Pts',(-1.94391746617626,-1.,-0.76349533353858));
#28948=CARTESIAN_POINT('Ctrl Pts',(-1.94391746617626,1.,-0.76349533353858));
#28949=CARTESIAN_POINT('Ctrl Pts',(-1.95015342590025,-1.,-0.762992990878774));
#28950=CARTESIAN_POINT('Ctrl Pts',(-1.95015342590025,1.,-0.762992990878774));
#28951=CARTESIAN_POINT('Ctrl Pts',(-1.95639665309893,-1.,-0.762447203806263));
#28952=CARTESIAN_POINT('Ctrl Pts',(-1.95639665309893,1.,-0.762447203806263));
#28953=CARTESIAN_POINT('Ctrl Pts',(-1.96264672744229,-1.,-0.761858300014575));
#28954=CARTESIAN_POINT('Ctrl Pts',(-1.96264672744229,1.,-0.761858300014575));
#28955=CARTESIAN_POINT('Ctrl Pts',(-1.96890351582545,-1.,-0.761226690483986));
#28956=CARTESIAN_POINT('Ctrl Pts',(-1.96890351582545,1.,-0.761226690483986));
#28957=CARTESIAN_POINT('Ctrl Pts',(-1.97516705321521,-1.,-0.760552825409855));
#28958=CARTESIAN_POINT('Ctrl Pts',(-1.97516705321521,1.,-0.760552825409855));
#28959=CARTESIAN_POINT('Ctrl Pts',(-1.98143741418156,-1.,-0.759837147452135));
#28960=CARTESIAN_POINT('Ctrl Pts',(-1.98143741418156,1.,-0.759837147452135));
#28961=CARTESIAN_POINT('Ctrl Pts',(-1.98771456680806,-1.,-0.759080037802242));
#28962=CARTESIAN_POINT('Ctrl Pts',(-1.98771456680806,1.,-0.759080037802242));
#28963=CARTESIAN_POINT('Ctrl Pts',(-1.9939983109871,-1.,-0.758281796766377));
#28964=CARTESIAN_POINT('Ctrl Pts',(-1.9939983109871,1.,-0.758281796766377));
#28965=CARTESIAN_POINT('Ctrl Pts',(-2.00028834739072,-1.,-0.757442676862341));
#28966=CARTESIAN_POINT('Ctrl Pts',(-2.00028834739072,1.,-0.757442676862341));
#28967=CARTESIAN_POINT('Ctrl Pts',(-2.00658431587682,-1.,-0.756562904646496));
#28968=CARTESIAN_POINT('Ctrl Pts',(-2.00658431587682,1.,-0.756562904646496));
#28969=CARTESIAN_POINT('Ctrl Pts',(-2.01288584328149,-1.,-0.7556427049581));
#28970=CARTESIAN_POINT('Ctrl Pts',(-2.01288584328149,1.,-0.7556427049581));
#28971=CARTESIAN_POINT('Ctrl Pts',(-2.01919259406003,-1.,-0.75468233072352));
#28972=CARTESIAN_POINT('Ctrl Pts',(-2.01919259406003,1.,-0.75468233072352));
#28973=CARTESIAN_POINT('Ctrl Pts',(-2.02550428623587,-1.,-0.753682061113765));
#28974=CARTESIAN_POINT('Ctrl Pts',(-2.02550428623587,1.,-0.753682061113765));
#28975=CARTESIAN_POINT('Ctrl Pts',(-2.03182068456467,-1.,-0.752642180488104));
#28976=CARTESIAN_POINT('Ctrl Pts',(-2.03182068456467,1.,-0.752642180488104));
#28977=CARTESIAN_POINT('Ctrl Pts',(-2.03814160092173,-1.,-0.751562963361383));
#28978=CARTESIAN_POINT('Ctrl Pts',(-2.03814160092173,1.,-0.751562963361383));
#28979=CARTESIAN_POINT('Ctrl Pts',(-2.04446689147754,-1.,-0.750444657874758));
#28980=CARTESIAN_POINT('Ctrl Pts',(-2.04446689147754,1.,-0.750444657874758));
#28981=CARTESIAN_POINT('Ctrl Pts',(-2.05079645591606,-1.,-0.749287468663053));
#28982=CARTESIAN_POINT('Ctrl Pts',(-2.05079645591606,1.,-0.749287468663053));
#28983=CARTESIAN_POINT('Ctrl Pts',(-2.05713023030263,-1.,-0.748091554181101));
#28984=CARTESIAN_POINT('Ctrl Pts',(-2.05713023030263,1.,-0.748091554181101));
#28985=CARTESIAN_POINT('Ctrl Pts',(-2.06220058927162,-1.,-0.747103932785504));
#28986=CARTESIAN_POINT('Ctrl Pts',(-2.06220058927162,1.,-0.747103932785504));
#28987=CARTESIAN_POINT('Ctrl Pts',(-2.06600523016401,-1.,-0.746345871542695));
#28988=CARTESIAN_POINT('Ctrl Pts',(-2.06600523016401,1.,-0.746345871542695));
#28989=CARTESIAN_POINT('Ctrl Pts',(-2.06854248895575,-1.,-0.74583279137781));
#28990=CARTESIAN_POINT('Ctrl Pts',(-2.06854248895575,1.,-0.74583279137781));
#28991=CARTESIAN_POINT('Ctrl Pts',(-2.0698113262342,-1.,-0.745574324794401));
#28992=CARTESIAN_POINT('Ctrl Pts',(-2.0698113262342,1.,-0.745574324794401));
#28993=CARTESIAN_POINT('',(-1.60662857109684,1.,-0.693717979106306));
#28994=CARTESIAN_POINT('Ctrl Pts',(-1.60662857109684,1.,-0.693717979106306));
#28995=CARTESIAN_POINT('Ctrl Pts',(-1.61106790958151,1.,-0.695712097881194));
#28996=CARTESIAN_POINT('Ctrl Pts',(-1.61974673472612,1.,-0.699605146405088));
#28997=CARTESIAN_POINT('Ctrl Pts',(-1.63216541664676,1.,-0.705159151988319));
#28998=CARTESIAN_POINT('Ctrl Pts',(-1.64752408832016,1.,-0.711993139355394));
#28999=CARTESIAN_POINT('Ctrl Pts',(-1.6647288055568,1.,-0.719585433804282));
#29000=CARTESIAN_POINT('Ctrl Pts',(-1.67996158455503,1.,-0.726235967997433));
#29001=CARTESIAN_POINT('Ctrl Pts',(-1.69326921975743,1.,-0.731963238697195));
#29002=CARTESIAN_POINT('Ctrl Pts',(-1.70473309006121,1.,-0.736799665724771));
#29003=CARTESIAN_POINT('Ctrl Pts',(-1.71447789751927,1.,-0.740795162032087));
#29004=CARTESIAN_POINT('Ctrl Pts',(-1.7226822991693,1.,-0.744021445433764));
#29005=CARTESIAN_POINT('Ctrl Pts',(-1.72958533647399,1.,-0.746574710096436));
#29006=CARTESIAN_POINT('Ctrl Pts',(-1.73550351679848,1.,-0.748582462954854));
#29007=CARTESIAN_POINT('Ctrl Pts',(-1.74080458266705,1.,-0.75019343597954));
#29008=CARTESIAN_POINT('Ctrl Pts',(-1.74585086852298,1.,-0.751555614163629));
#29009=CARTESIAN_POINT('Ctrl Pts',(-1.75095139468809,1.,-0.752797683531377));
#29010=CARTESIAN_POINT('Ctrl Pts',(-1.75631083600175,1.,-0.75400925402848));
#29011=CARTESIAN_POINT('Ctrl Pts',(-1.7619781724032,1.,-0.755220979975262));
#29012=CARTESIAN_POINT('Ctrl Pts',(-1.76789396003141,1.,-0.756421896028403));
#29013=CARTESIAN_POINT('Ctrl Pts',(-1.77394167108342,1.,-0.757578264077238));
#29014=CARTESIAN_POINT('Ctrl Pts',(-1.77999411220912,1.,-0.75865062667738));
#29015=CARTESIAN_POINT('Ctrl Pts',(-1.78596964884526,1.,-0.759614401109868));
#29016=CARTESIAN_POINT('Ctrl Pts',(-1.79185815610802,1.,-0.760469555880425));
#29017=CARTESIAN_POINT('Ctrl Pts',(-1.79768986997735,1.,-0.761229695230359));
#29018=CARTESIAN_POINT('Ctrl Pts',(-1.80351583877334,1.,-0.761915336443515));
#29019=CARTESIAN_POINT('Ctrl Pts',(-1.80938551463989,1.,-0.762546129464036));
#29020=CARTESIAN_POINT('Ctrl Pts',(-1.81532118405566,1.,-0.763132003836783));
#29021=CARTESIAN_POINT('Ctrl Pts',(-1.82131873145297,1.,-0.763673465462854));
#29022=CARTESIAN_POINT('Ctrl Pts',(-1.8273599120008,1.,-0.764165902606055));
#29023=CARTESIAN_POINT('Ctrl Pts',(-1.8334207722714,1.,-0.764602549687845));
#29024=CARTESIAN_POINT('Ctrl Pts',(-1.83948181064823,1.,-0.764978057881687));
#29025=CARTESIAN_POINT('Ctrl Pts',(-1.8455369887591,1.,-0.765291664861971));
#29026=CARTESIAN_POINT('Ctrl Pts',(-1.85158945130054,1.,-0.765545710619023));
#29027=CARTESIAN_POINT('Ctrl Pts',(-1.85764741390391,1.,-0.765744212909305));
#29028=CARTESIAN_POINT('Ctrl Pts',(-1.86372027063314,1.,-0.765891519092557));
#29029=CARTESIAN_POINT('Ctrl Pts',(-1.86981398314345,1.,-0.765990708546111));
#29030=CARTESIAN_POINT('Ctrl Pts',(-1.87592888967886,1.,-0.766042837036759));
#29031=CARTESIAN_POINT('Ctrl Pts',(-1.88206215302561,1.,-0.766047794851868));
#29032=CARTESIAN_POINT('Ctrl Pts',(-1.88820926433409,1.,-0.76600483706209));
#29033=CARTESIAN_POINT('Ctrl Pts',(-1.89436577771389,1.,-0.765913193856979));
#29034=CARTESIAN_POINT('Ctrl Pts',(-1.90052930393599,1.,-0.765772772593395));
#29035=CARTESIAN_POINT('Ctrl Pts',(-1.90669961402362,1.,-0.765584196937936));
#29036=CARTESIAN_POINT('Ctrl Pts',(-1.91287765805174,1.,-0.765348465884739));
#29037=CARTESIAN_POINT('Ctrl Pts',(-1.91906491634197,1.,-0.765066729667095));
#29038=CARTESIAN_POINT('Ctrl Pts',(-1.92526263537041,1.,-0.764740025488189));
#29039=CARTESIAN_POINT('Ctrl Pts',(-1.93147105496367,1.,-0.764369010673889));
#29040=CARTESIAN_POINT('Ctrl Pts',(-1.93768964875867,1.,-0.763954049121393));
#29041=CARTESIAN_POINT('Ctrl Pts',(-1.94391746617626,1.,-0.76349533353858));
#29042=CARTESIAN_POINT('Ctrl Pts',(-1.95015342590025,1.,-0.762992990878774));
#29043=CARTESIAN_POINT('Ctrl Pts',(-1.95639665309893,1.,-0.762447203806263));
#29044=CARTESIAN_POINT('Ctrl Pts',(-1.96264672744229,1.,-0.761858300014575));
#29045=CARTESIAN_POINT('Ctrl Pts',(-1.96890351582545,1.,-0.761226690483986));
#29046=CARTESIAN_POINT('Ctrl Pts',(-1.97516705321521,1.,-0.760552825409855));
#29047=CARTESIAN_POINT('Ctrl Pts',(-1.98143741418156,1.,-0.759837147452135));
#29048=CARTESIAN_POINT('Ctrl Pts',(-1.98771456680806,1.,-0.759080037802242));
#29049=CARTESIAN_POINT('Ctrl Pts',(-1.9939983109871,1.,-0.758281796766377));
#29050=CARTESIAN_POINT('Ctrl Pts',(-2.00028834739072,1.,-0.757442676862341));
#29051=CARTESIAN_POINT('Ctrl Pts',(-2.00658431587682,1.,-0.756562904646496));
#29052=CARTESIAN_POINT('Ctrl Pts',(-2.01288584328149,1.,-0.7556427049581));
#29053=CARTESIAN_POINT('Ctrl Pts',(-2.01919259406003,1.,-0.75468233072352));
#29054=CARTESIAN_POINT('Ctrl Pts',(-2.02550428623587,1.,-0.753682061113765));
#29055=CARTESIAN_POINT('Ctrl Pts',(-2.03182068456467,1.,-0.752642180488104));
#29056=CARTESIAN_POINT('Ctrl Pts',(-2.03814160092173,1.,-0.751562963361383));
#29057=CARTESIAN_POINT('Ctrl Pts',(-2.04446689147754,1.,-0.750444657874758));
#29058=CARTESIAN_POINT('Ctrl Pts',(-2.05079645591606,1.,-0.749287468663053));
#29059=CARTESIAN_POINT('Ctrl Pts',(-2.05713023030263,1.,-0.748091554181101));
#29060=CARTESIAN_POINT('Ctrl Pts',(-2.06220058927162,1.,-0.747103932785504));
#29061=CARTESIAN_POINT('Ctrl Pts',(-2.06600523016401,1.,-0.746345871542695));
#29062=CARTESIAN_POINT('Ctrl Pts',(-2.06854248895575,1.,-0.74583279137781));
#29063=CARTESIAN_POINT('Ctrl Pts',(-2.0698113262342,1.,-0.745574324794401));
#29064=CARTESIAN_POINT('',(-1.60662857109684,0.,-0.693717979106306));
#29065=CARTESIAN_POINT('Origin',(0.,0.,0.));
#29066=CARTESIAN_POINT('',(-1.5055822144029,1.,-0.892032620296855));
#29067=CARTESIAN_POINT('Origin',(0.,1.,0.));
#29068=CARTESIAN_POINT('',(-1.5055822144029,0.,-0.892032620296855));
#29069=CARTESIAN_POINT('Ctrl Pts',(-1.81978687191668,-1.,-1.23627494547115));
#29070=CARTESIAN_POINT('Ctrl Pts',(-1.81978687191668,1.,-1.23627494547115));
#29071=CARTESIAN_POINT('Ctrl Pts',(-1.81925017193666,-1.,-1.23509651170476));
#29072=CARTESIAN_POINT('Ctrl Pts',(-1.81925017193666,1.,-1.23509651170476));
#29073=CARTESIAN_POINT('Ctrl Pts',(-1.81817389921279,-1.,-1.2327422452705));
#29074=CARTESIAN_POINT('Ctrl Pts',(-1.81817389921279,1.,-1.2327422452705));
#29075=CARTESIAN_POINT('Ctrl Pts',(-1.8165508718364,-1.,-1.2292186489137));
#29076=CARTESIAN_POINT('Ctrl Pts',(-1.8165508718364,1.,-1.2292186489137));
#29077=CARTESIAN_POINT('Ctrl Pts',(-1.81436959210434,-1.,-1.2245361330495));
#29078=CARTESIAN_POINT('Ctrl Pts',(-1.81436959210434,1.,-1.2245361330495));
#29079=CARTESIAN_POINT('Ctrl Pts',(-1.81161420806656,-1.,-1.21870906103557));
#29080=CARTESIAN_POINT('Ctrl Pts',(-1.81161420806656,1.,-1.21870906103557));
#29081=CARTESIAN_POINT('Ctrl Pts',(-1.80882996917129,-1.,-1.21290815708314));
#29082=CARTESIAN_POINT('Ctrl Pts',(-1.80882996917129,1.,-1.21290815708314));
#29083=CARTESIAN_POINT('Ctrl Pts',(-1.80601678480707,-1.,-1.20713356605475));
#29084=CARTESIAN_POINT('Ctrl Pts',(-1.80601678480707,1.,-1.20713356605475));
#29085=CARTESIAN_POINT('Ctrl Pts',(-1.80317454838603,-1.,-1.20138548938974));
#29086=CARTESIAN_POINT('Ctrl Pts',(-1.80317454838603,1.,-1.20138548938974));
#29087=CARTESIAN_POINT('Ctrl Pts',(-1.80030314369879,-1.,-1.19566418930242));
#29088=CARTESIAN_POINT('Ctrl Pts',(-1.80030314369879,1.,-1.19566418930242));
#29089=CARTESIAN_POINT('Ctrl Pts',(-1.79740245923478,-1.,-1.18996997934445));
#29090=CARTESIAN_POINT('Ctrl Pts',(-1.79740245923478,1.,-1.18996997934445));
#29091=CARTESIAN_POINT('Ctrl Pts',(-1.79447240321515,-1.,-1.18430321697432));
#29092=CARTESIAN_POINT('Ctrl Pts',(-1.79447240321515,1.,-1.18430321697432));
#29093=CARTESIAN_POINT('Ctrl Pts',(-1.79151291552689,-1.,-1.17866429440809));
#29094=CARTESIAN_POINT('Ctrl Pts',(-1.79151291552689,1.,-1.17866429440809));
#29095=CARTESIAN_POINT('Ctrl Pts',(-1.78852398877616,-1.,-1.17305363177328));
#29096=CARTESIAN_POINT('Ctrl Pts',(-1.78852398877616,1.,-1.17305363177328));
#29097=CARTESIAN_POINT('Ctrl Pts',(-1.78550566040443,-1.,-1.16747166312303));
#29098=CARTESIAN_POINT('Ctrl Pts',(-1.78550566040443,1.,-1.16747166312303));
#29099=CARTESIAN_POINT('Ctrl Pts',(-1.78245795881009,-1.,-1.16191881298499));
#29100=CARTESIAN_POINT('Ctrl Pts',(-1.78245795881009,1.,-1.16191881298499));
#29101=CARTESIAN_POINT('Ctrl Pts',(-1.77938085564275,-1.,-1.15639547194698));
#29102=CARTESIAN_POINT('Ctrl Pts',(-1.77938085564275,1.,-1.15639547194698));
#29103=CARTESIAN_POINT('Ctrl Pts',(-1.7762742255701,-1.,-1.15090197841515));
#29104=CARTESIAN_POINT('Ctrl Pts',(-1.7762742255701,1.,-1.15090197841515));
#29105=CARTESIAN_POINT('Ctrl Pts',(-1.77313777896194,-1.,-1.1454385822692));
#29106=CARTESIAN_POINT('Ctrl Pts',(-1.77313777896194,1.,-1.1454385822692));
#29107=CARTESIAN_POINT('Ctrl Pts',(-1.76997111386769,-1.,-1.14000548336975));
#29108=CARTESIAN_POINT('Ctrl Pts',(-1.76997111386769,1.,-1.14000548336975));
#29109=CARTESIAN_POINT('Ctrl Pts',(-1.76677384551862,-1.,-1.1346029180462));
#29110=CARTESIAN_POINT('Ctrl Pts',(-1.76677384551862,1.,-1.1346029180462));
#29111=CARTESIAN_POINT('Ctrl Pts',(-1.7635457196617,-1.,-1.12923123555075));
#29112=CARTESIAN_POINT('Ctrl Pts',(-1.7635457196617,1.,-1.12923123555075));
#29113=CARTESIAN_POINT('Ctrl Pts',(-1.76028671825096,-1.,-1.12389096855086));
#29114=CARTESIAN_POINT('Ctrl Pts',(-1.76028671825096,1.,-1.12389096855086));
#29115=CARTESIAN_POINT('Ctrl Pts',(-1.75699720772105,-1.,-1.11858293216763));
#29116=CARTESIAN_POINT('Ctrl Pts',(-1.75699720772105,1.,-1.11858293216763));
#29117=CARTESIAN_POINT('Ctrl Pts',(-1.7536777209463,-1.,-1.11330807582551));
#29118=CARTESIAN_POINT('Ctrl Pts',(-1.7536777209463,1.,-1.11330807582551));
#29119=CARTESIAN_POINT('Ctrl Pts',(-1.7503286607592,-1.,-1.10806728183007));
#29120=CARTESIAN_POINT('Ctrl Pts',(-1.7503286607592,1.,-1.10806728183007));
#29121=CARTESIAN_POINT('Ctrl Pts',(-1.74695004214923,-1.,-1.10286118991143));
#29122=CARTESIAN_POINT('Ctrl Pts',(-1.74695004214923,1.,-1.10286118991143));
#29123=CARTESIAN_POINT('Ctrl Pts',(-1.74354119236208,-1.,-1.09768999241225));
#29124=CARTESIAN_POINT('Ctrl Pts',(-1.74354119236208,1.,-1.09768999241225));
#29125=CARTESIAN_POINT('Ctrl Pts',(-1.74010053962247,-1.,-1.09255329056493));
#29126=CARTESIAN_POINT('Ctrl Pts',(-1.74010053962247,1.,-1.09255329056493));
#29127=CARTESIAN_POINT('Ctrl Pts',(-1.73662628326091,-1.,-1.08745056285427));
#29128=CARTESIAN_POINT('Ctrl Pts',(-1.73662628326091,1.,-1.08745056285427));
#29129=CARTESIAN_POINT('Ctrl Pts',(-1.73311705663407,-1.,-1.08238162784749));
#29130=CARTESIAN_POINT('Ctrl Pts',(-1.73311705663407,1.,-1.08238162784749));
#29131=CARTESIAN_POINT('Ctrl Pts',(-1.72957248977424,-1.,-1.0773470373727));
#29132=CARTESIAN_POINT('Ctrl Pts',(-1.72957248977424,1.,-1.0773470373727));
#29133=CARTESIAN_POINT('Ctrl Pts',(-1.72599406198488,-1.,-1.07234866990252));
#29134=CARTESIAN_POINT('Ctrl Pts',(-1.72599406198488,1.,-1.07234866990252));
#29135=CARTESIAN_POINT('Ctrl Pts',(-1.72238500928453,-1.,-1.06738966975462));
#29136=CARTESIAN_POINT('Ctrl Pts',(-1.72238500928453,1.,-1.06738966975462));
#29137=CARTESIAN_POINT('Ctrl Pts',(-1.71874858456904,-1.,-1.06247324680647));
#29138=CARTESIAN_POINT('Ctrl Pts',(-1.71874858456904,1.,-1.06247324680647));
#29139=CARTESIAN_POINT('Ctrl Pts',(-1.7150865442702,-1.,-1.05760163192479));
#29140=CARTESIAN_POINT('Ctrl Pts',(-1.7150865442702,1.,-1.05760163192479));
#29141=CARTESIAN_POINT('Ctrl Pts',(-1.71139783543989,-1.,-1.05277517202855));
#29142=CARTESIAN_POINT('Ctrl Pts',(-1.71139783543989,1.,-1.05277517202855));
#29143=CARTESIAN_POINT('Ctrl Pts',(-1.70767646263649,-1.,-1.04799085404995));
#29144=CARTESIAN_POINT('Ctrl Pts',(-1.70767646263649,1.,-1.04799085404995));
#29145=CARTESIAN_POINT('Ctrl Pts',(-1.70391338707982,-1.,-1.04324363334554));
#29146=CARTESIAN_POINT('Ctrl Pts',(-1.70391338707982,1.,-1.04324363334554));
#29147=CARTESIAN_POINT('Ctrl Pts',(-1.70010052930962,-1.,-1.03852922490789));
#29148=CARTESIAN_POINT('Ctrl Pts',(-1.70010052930962,1.,-1.03852922490789));
#29149=CARTESIAN_POINT('Ctrl Pts',(-1.69623414782771,-1.,-1.03384646003588));
#29150=CARTESIAN_POINT('Ctrl Pts',(-1.69623414782771,1.,-1.03384646003588));
#29151=CARTESIAN_POINT('Ctrl Pts',(-1.69231840863458,-1.,-1.02919977579147));
#29152=CARTESIAN_POINT('Ctrl Pts',(-1.69231840863458,1.,-1.02919977579147));
#29153=CARTESIAN_POINT('Ctrl Pts',(-1.68836910178447,-1.,-1.02460180535255));
#29154=CARTESIAN_POINT('Ctrl Pts',(-1.68836910178447,1.,-1.02460180535255));
#29155=CARTESIAN_POINT('Ctrl Pts',(-1.68440578021706,-1.,-1.02006795074201));
#29156=CARTESIAN_POINT('Ctrl Pts',(-1.68440578021706,1.,-1.02006795074201));
#29157=CARTESIAN_POINT('Ctrl Pts',(-1.68044289894798,-1.,-1.01561026162773));
#29158=CARTESIAN_POINT('Ctrl Pts',(-1.68044289894798,1.,-1.01561026162773));
#29159=CARTESIAN_POINT('Ctrl Pts',(-1.67648246776464,-1.,-1.01123236493511));
#29160=CARTESIAN_POINT('Ctrl Pts',(-1.67648246776464,1.,-1.01123236493511));
#29161=CARTESIAN_POINT('Ctrl Pts',(-1.67250335383293,-1.,-1.00692206696414));
#29162=CARTESIAN_POINT('Ctrl Pts',(-1.67250335383293,1.,-1.00692206696414));
#29163=CARTESIAN_POINT('Ctrl Pts',(-1.66846059277303,-1.,-1.00265091003727));
#29164=CARTESIAN_POINT('Ctrl Pts',(-1.66846059277303,1.,-1.00265091003727));
#29165=CARTESIAN_POINT('Ctrl Pts',(-1.66430758030376,-1.,-0.998389654952758));
#29166=CARTESIAN_POINT('Ctrl Pts',(-1.66430758030376,1.,-0.998389654952758));
#29167=CARTESIAN_POINT('Ctrl Pts',(-1.66001553809947,-1.,-0.994121836661306));
#29168=CARTESIAN_POINT('Ctrl Pts',(-1.66001553809947,1.,-0.994121836661306));
#29169=CARTESIAN_POINT('Ctrl Pts',(-1.65559044289699,-1.,-0.989855627854165));
#29170=CARTESIAN_POINT('Ctrl Pts',(-1.65559044289699,1.,-0.989855627854165));
#29171=CARTESIAN_POINT('Ctrl Pts',(-1.65110016612638,-1.,-0.985642622920821));
#29172=CARTESIAN_POINT('Ctrl Pts',(-1.65110016612638,1.,-0.985642622920821));
#29173=CARTESIAN_POINT('Ctrl Pts',(-1.64665139190656,-1.,-0.981562530939489));
#29174=CARTESIAN_POINT('Ctrl Pts',(-1.64665139190656,1.,-0.981562530939489));
#29175=CARTESIAN_POINT('Ctrl Pts',(-1.64233990826687,-1.,-0.977689794119416));
#29176=CARTESIAN_POINT('Ctrl Pts',(-1.64233990826687,1.,-0.977689794119416));
#29177=CARTESIAN_POINT('Ctrl Pts',(-1.63820952658144,-1.,-0.974066058287418));
#29178=CARTESIAN_POINT('Ctrl Pts',(-1.63820952658144,1.,-0.974066058287418));
#29179=CARTESIAN_POINT('Ctrl Pts',(-1.63420665729798,-1.,-0.970669715997509));
#29180=CARTESIAN_POINT('Ctrl Pts',(-1.63420665729798,1.,-0.970669715997509));
#29181=CARTESIAN_POINT('Ctrl Pts',(-1.63013849959461,-1.,-0.967387853230345));
#29182=CARTESIAN_POINT('Ctrl Pts',(-1.63013849959461,1.,-0.967387853230345));
#29183=CARTESIAN_POINT('Ctrl Pts',(-1.62571930670187,-1.,-0.964046107040536));
#29184=CARTESIAN_POINT('Ctrl Pts',(-1.62571930670187,1.,-0.964046107040536));
#29185=CARTESIAN_POINT('Ctrl Pts',(-1.62061638140221,-1.,-0.960438326101729));
#29186=CARTESIAN_POINT('Ctrl Pts',(-1.62061638140221,1.,-0.960438326101729));
#29187=CARTESIAN_POINT('Ctrl Pts',(-1.61449324337085,-1.,-0.956354422920671));
#29188=CARTESIAN_POINT('Ctrl Pts',(-1.61449324337085,1.,-0.956354422920671));
#29189=CARTESIAN_POINT('Ctrl Pts',(-1.60706069896936,-1.,-0.951613284356035));
#29190=CARTESIAN_POINT('Ctrl Pts',(-1.60706069896936,1.,-0.951613284356035));
#29191=CARTESIAN_POINT('Ctrl Pts',(-1.59810042043673,-1.,-0.946078063315257));
#29192=CARTESIAN_POINT('Ctrl Pts',(-1.59810042043673,1.,-0.946078063315257));
#29193=CARTESIAN_POINT('Ctrl Pts',(-1.58744937487176,-1.,-0.939646377893399));
#29194=CARTESIAN_POINT('Ctrl Pts',(-1.58744937487176,1.,-0.939646377893399));
#29195=CARTESIAN_POINT('Ctrl Pts',(-1.57499388382243,-1.,-0.932246680108685));
#29196=CARTESIAN_POINT('Ctrl Pts',(-1.57499388382243,1.,-0.932246680108685));
#29197=CARTESIAN_POINT('Ctrl Pts',(-1.56065988578893,-1.,-0.923832188944341));
#29198=CARTESIAN_POINT('Ctrl Pts',(-1.56065988578893,1.,-0.923832188944341));
#29199=CARTESIAN_POINT('Ctrl Pts',(-1.54440491149498,-1.,-0.914375919026456));
#29200=CARTESIAN_POINT('Ctrl Pts',(-1.54440491149498,1.,-0.914375919026456));
#29201=CARTESIAN_POINT('Ctrl Pts',(-1.52984849887993,-1.,-0.905967409625651));
#29202=CARTESIAN_POINT('Ctrl Pts',(-1.52984849887993,1.,-0.905967409625651));
#29203=CARTESIAN_POINT('Ctrl Pts',(-1.51805569590094,-1.,-0.899185047483511));
#29204=CARTESIAN_POINT('Ctrl Pts',(-1.51805569590094,1.,-0.899185047483511));
#29205=CARTESIAN_POINT('Ctrl Pts',(-1.50980486806688,-1.,-0.894452006964543));
#29206=CARTESIAN_POINT('Ctrl Pts',(-1.50980486806688,1.,-0.894452006964543));
#29207=CARTESIAN_POINT('Ctrl Pts',(-1.5055822144029,-1.,-0.892032620296855));
#29208=CARTESIAN_POINT('Ctrl Pts',(-1.5055822144029,1.,-0.892032620296855));
#29209=CARTESIAN_POINT('',(-1.81978687191668,1.,-1.23627494547115));
#29210=CARTESIAN_POINT('Ctrl Pts',(-1.81978687191668,1.,-1.23627494547115));
#29211=CARTESIAN_POINT('Ctrl Pts',(-1.81925017193666,1.,-1.23509651170476));
#29212=CARTESIAN_POINT('Ctrl Pts',(-1.81817389921279,1.,-1.2327422452705));
#29213=CARTESIAN_POINT('Ctrl Pts',(-1.8165508718364,1.,-1.2292186489137));
#29214=CARTESIAN_POINT('Ctrl Pts',(-1.81436959210434,1.,-1.2245361330495));
#29215=CARTESIAN_POINT('Ctrl Pts',(-1.81161420806656,1.,-1.21870906103557));
#29216=CARTESIAN_POINT('Ctrl Pts',(-1.80882996917129,1.,-1.21290815708314));
#29217=CARTESIAN_POINT('Ctrl Pts',(-1.80601678480707,1.,-1.20713356605475));
#29218=CARTESIAN_POINT('Ctrl Pts',(-1.80317454838603,1.,-1.20138548938974));
#29219=CARTESIAN_POINT('Ctrl Pts',(-1.80030314369879,1.,-1.19566418930242));
#29220=CARTESIAN_POINT('Ctrl Pts',(-1.79740245923478,1.,-1.18996997934445));
#29221=CARTESIAN_POINT('Ctrl Pts',(-1.79447240321515,1.,-1.18430321697432));
#29222=CARTESIAN_POINT('Ctrl Pts',(-1.79151291552689,1.,-1.17866429440809));
#29223=CARTESIAN_POINT('Ctrl Pts',(-1.78852398877616,1.,-1.17305363177328));
#29224=CARTESIAN_POINT('Ctrl Pts',(-1.78550566040443,1.,-1.16747166312303));
#29225=CARTESIAN_POINT('Ctrl Pts',(-1.78245795881009,1.,-1.16191881298499));
#29226=CARTESIAN_POINT('Ctrl Pts',(-1.77938085564275,1.,-1.15639547194698));
#29227=CARTESIAN_POINT('Ctrl Pts',(-1.7762742255701,1.,-1.15090197841515));
#29228=CARTESIAN_POINT('Ctrl Pts',(-1.77313777896194,1.,-1.1454385822692));
#29229=CARTESIAN_POINT('Ctrl Pts',(-1.76997111386769,1.,-1.14000548336975));
#29230=CARTESIAN_POINT('Ctrl Pts',(-1.76677384551862,1.,-1.1346029180462));
#29231=CARTESIAN_POINT('Ctrl Pts',(-1.7635457196617,1.,-1.12923123555075));
#29232=CARTESIAN_POINT('Ctrl Pts',(-1.76028671825096,1.,-1.12389096855086));
#29233=CARTESIAN_POINT('Ctrl Pts',(-1.75699720772105,1.,-1.11858293216763));
#29234=CARTESIAN_POINT('Ctrl Pts',(-1.7536777209463,1.,-1.11330807582551));
#29235=CARTESIAN_POINT('Ctrl Pts',(-1.7503286607592,1.,-1.10806728183007));
#29236=CARTESIAN_POINT('Ctrl Pts',(-1.74695004214923,1.,-1.10286118991143));
#29237=CARTESIAN_POINT('Ctrl Pts',(-1.74354119236208,1.,-1.09768999241225));
#29238=CARTESIAN_POINT('Ctrl Pts',(-1.74010053962247,1.,-1.09255329056493));
#29239=CARTESIAN_POINT('Ctrl Pts',(-1.73662628326091,1.,-1.08745056285427));
#29240=CARTESIAN_POINT('Ctrl Pts',(-1.73311705663407,1.,-1.08238162784749));
#29241=CARTESIAN_POINT('Ctrl Pts',(-1.72957248977424,1.,-1.0773470373727));
#29242=CARTESIAN_POINT('Ctrl Pts',(-1.72599406198488,1.,-1.07234866990252));
#29243=CARTESIAN_POINT('Ctrl Pts',(-1.72238500928453,1.,-1.06738966975462));
#29244=CARTESIAN_POINT('Ctrl Pts',(-1.71874858456904,1.,-1.06247324680647));
#29245=CARTESIAN_POINT('Ctrl Pts',(-1.7150865442702,1.,-1.05760163192479));
#29246=CARTESIAN_POINT('Ctrl Pts',(-1.71139783543989,1.,-1.05277517202855));
#29247=CARTESIAN_POINT('Ctrl Pts',(-1.70767646263649,1.,-1.04799085404995));
#29248=CARTESIAN_POINT('Ctrl Pts',(-1.70391338707982,1.,-1.04324363334554));
#29249=CARTESIAN_POINT('Ctrl Pts',(-1.70010052930962,1.,-1.03852922490789));
#29250=CARTESIAN_POINT('Ctrl Pts',(-1.69623414782771,1.,-1.03384646003588));
#29251=CARTESIAN_POINT('Ctrl Pts',(-1.69231840863458,1.,-1.02919977579147));
#29252=CARTESIAN_POINT('Ctrl Pts',(-1.68836910178447,1.,-1.02460180535255));
#29253=CARTESIAN_POINT('Ctrl Pts',(-1.68440578021706,1.,-1.02006795074201));
#29254=CARTESIAN_POINT('Ctrl Pts',(-1.68044289894798,1.,-1.01561026162773));
#29255=CARTESIAN_POINT('Ctrl Pts',(-1.67648246776464,1.,-1.01123236493511));
#29256=CARTESIAN_POINT('Ctrl Pts',(-1.67250335383293,1.,-1.00692206696414));
#29257=CARTESIAN_POINT('Ctrl Pts',(-1.66846059277303,1.,-1.00265091003727));
#29258=CARTESIAN_POINT('Ctrl Pts',(-1.66430758030376,1.,-0.998389654952758));
#29259=CARTESIAN_POINT('Ctrl Pts',(-1.66001553809947,1.,-0.994121836661306));
#29260=CARTESIAN_POINT('Ctrl Pts',(-1.65559044289699,1.,-0.989855627854165));
#29261=CARTESIAN_POINT('Ctrl Pts',(-1.65110016612638,1.,-0.985642622920821));
#29262=CARTESIAN_POINT('Ctrl Pts',(-1.64665139190656,1.,-0.981562530939489));
#29263=CARTESIAN_POINT('Ctrl Pts',(-1.64233990826687,1.,-0.977689794119416));
#29264=CARTESIAN_POINT('Ctrl Pts',(-1.63820952658144,1.,-0.974066058287418));
#29265=CARTESIAN_POINT('Ctrl Pts',(-1.63420665729798,1.,-0.970669715997509));
#29266=CARTESIAN_POINT('Ctrl Pts',(-1.63013849959461,1.,-0.967387853230345));
#29267=CARTESIAN_POINT('Ctrl Pts',(-1.62571930670187,1.,-0.964046107040536));
#29268=CARTESIAN_POINT('Ctrl Pts',(-1.62061638140221,1.,-0.960438326101729));
#29269=CARTESIAN_POINT('Ctrl Pts',(-1.61449324337085,1.,-0.956354422920671));
#29270=CARTESIAN_POINT('Ctrl Pts',(-1.60706069896936,1.,-0.951613284356035));
#29271=CARTESIAN_POINT('Ctrl Pts',(-1.59810042043673,1.,-0.946078063315257));
#29272=CARTESIAN_POINT('Ctrl Pts',(-1.58744937487176,1.,-0.939646377893399));
#29273=CARTESIAN_POINT('Ctrl Pts',(-1.57499388382243,1.,-0.932246680108685));
#29274=CARTESIAN_POINT('Ctrl Pts',(-1.56065988578893,1.,-0.923832188944341));
#29275=CARTESIAN_POINT('Ctrl Pts',(-1.54440491149498,1.,-0.914375919026456));
#29276=CARTESIAN_POINT('Ctrl Pts',(-1.52984849887993,1.,-0.905967409625651));
#29277=CARTESIAN_POINT('Ctrl Pts',(-1.51805569590094,1.,-0.899185047483511));
#29278=CARTESIAN_POINT('Ctrl Pts',(-1.50980486806688,1.,-0.894452006964543));
#29279=CARTESIAN_POINT('Ctrl Pts',(-1.5055822144029,1.,-0.892032620296855));
#29280=CARTESIAN_POINT('',(-1.81978687191668,0.,-1.23627494547115));
#29281=CARTESIAN_POINT('Origin',(-1.73811241238545,0.,-1.34869019493419));
#29282=CARTESIAN_POINT('',(-1.73811241238545,1.,-1.34869019493419));
#29283=CARTESIAN_POINT('',(-1.81978687191668,1.,-1.23627494547115));
#29284=CARTESIAN_POINT('',(-1.73811241238545,0.,-1.34869019493419));
#29285=CARTESIAN_POINT('Ctrl Pts',(-1.31362392696032,-1.,-1.15624053661742));
#29286=CARTESIAN_POINT('Ctrl Pts',(-1.31362392696032,1.,-1.15624053661742));
#29287=CARTESIAN_POINT('Ctrl Pts',(-1.31722977216397,-1.,-1.15950888730809));
#29288=CARTESIAN_POINT('Ctrl Pts',(-1.31722977216397,1.,-1.15950888730809));
#29289=CARTESIAN_POINT('Ctrl Pts',(-1.32428080721772,-1.,-1.16589330093588));
#29290=CARTESIAN_POINT('Ctrl Pts',(-1.32428080721772,1.,-1.16589330093588));
#29291=CARTESIAN_POINT('Ctrl Pts',(-1.33437539347008,-1.,-1.17501305789857));
#29292=CARTESIAN_POINT('Ctrl Pts',(-1.33437539347008,1.,-1.17501305789857));
#29293=CARTESIAN_POINT('Ctrl Pts',(-1.34687054001093,-1.,-1.18625865667441));
#29294=CARTESIAN_POINT('Ctrl Pts',(-1.34687054001093,1.,-1.18625865667441));
#29295=CARTESIAN_POINT('Ctrl Pts',(-1.36088705043885,-1.,-1.1987959077932));
#29296=CARTESIAN_POINT('Ctrl Pts',(-1.36088705043885,1.,-1.1987959077932));
#29297=CARTESIAN_POINT('Ctrl Pts',(-1.37331915607905,-1.,-1.20982812925645));
#29298=CARTESIAN_POINT('Ctrl Pts',(-1.37331915607905,1.,-1.20982812925645));
#29299=CARTESIAN_POINT('Ctrl Pts',(-1.38420564527715,-1.,-1.21938737280852));
#29300=CARTESIAN_POINT('Ctrl Pts',(-1.38420564527715,1.,-1.21938737280852));
#29301=CARTESIAN_POINT('Ctrl Pts',(-1.39361389568796,-1.,-1.22752961899387));
#29302=CARTESIAN_POINT('Ctrl Pts',(-1.39361389568796,1.,-1.22752961899387));
#29303=CARTESIAN_POINT('Ctrl Pts',(-1.40164708206106,-1.,-1.23434087290423));
#29304=CARTESIAN_POINT('Ctrl Pts',(-1.40164708206106,1.,-1.23434087290423));
#29305=CARTESIAN_POINT('Ctrl Pts',(-1.40845295531283,-1.,-1.23994455029534));
#29306=CARTESIAN_POINT('Ctrl Pts',(-1.40845295531283,1.,-1.23994455029534));
#29307=CARTESIAN_POINT('Ctrl Pts',(-1.41422913175179,-1.,-1.24450600513056));
#29308=CARTESIAN_POINT('Ctrl Pts',(-1.41422913175179,1.,-1.24450600513056));
#29309=CARTESIAN_POINT('Ctrl Pts',(-1.41923722596025,-1.,-1.24824430986571));
#29310=CARTESIAN_POINT('Ctrl Pts',(-1.41923722596025,1.,-1.24824430986571));
#29311=CARTESIAN_POINT('Ctrl Pts',(-1.42378102115575,-1.,-1.2514145557001));
#29312=CARTESIAN_POINT('Ctrl Pts',(-1.42378102115575,1.,-1.2514145557001));
#29313=CARTESIAN_POINT('Ctrl Pts',(-1.42815938799387,-1.,-1.25426945222639));
#29314=CARTESIAN_POINT('Ctrl Pts',(-1.42815938799387,1.,-1.25426945222639));
#29315=CARTESIAN_POINT('Ctrl Pts',(-1.43262645609691,-1.,-1.25702687965755));
#29316=CARTESIAN_POINT('Ctrl Pts',(-1.43262645609691,1.,-1.25702687965755));
#29317=CARTESIAN_POINT('Ctrl Pts',(-1.43734919180848,-1.,-1.25983531012005));
#29318=CARTESIAN_POINT('Ctrl Pts',(-1.43734919180848,1.,-1.25983531012005));
#29319=CARTESIAN_POINT('Ctrl Pts',(-1.44236470511303,-1.,-1.26273903323859));
#29320=CARTESIAN_POINT('Ctrl Pts',(-1.44236470511303,1.,-1.26273903323859));
#29321=CARTESIAN_POINT('Ctrl Pts',(-1.44761985001662,-1.,-1.26570925118868));
#29322=CARTESIAN_POINT('Ctrl Pts',(-1.44761985001662,1.,-1.26570925118868));
#29323=CARTESIAN_POINT('Ctrl Pts',(-1.45301422764247,-1.,-1.2686778680489));
#29324=CARTESIAN_POINT('Ctrl Pts',(-1.45301422764247,1.,-1.2686778680489));
#29325=CARTESIAN_POINT('Ctrl Pts',(-1.45843906294697,-1.,-1.27156805265289));
#29326=CARTESIAN_POINT('Ctrl Pts',(-1.45843906294697,1.,-1.27156805265289));
#29327=CARTESIAN_POINT('Ctrl Pts',(-1.46382431332476,-1.,-1.27433119897822));
#29328=CARTESIAN_POINT('Ctrl Pts',(-1.46382431332476,1.,-1.27433119897822));
#29329=CARTESIAN_POINT('Ctrl Pts',(-1.46916035917133,-1.,-1.27696414831089));
#29330=CARTESIAN_POINT('Ctrl Pts',(-1.46916035917133,1.,-1.27696414831089));
#29331=CARTESIAN_POINT('Ctrl Pts',(-1.4744717526707,-1.,-1.2794891824849));
#29332=CARTESIAN_POINT('Ctrl Pts',(-1.4744717526707,1.,-1.2794891824849));
#29333=CARTESIAN_POINT('Ctrl Pts',(-1.47980070347095,-1.,-1.28194158939517));
#29334=CARTESIAN_POINT('Ctrl Pts',(-1.47980070347095,1.,-1.28194158939517));
#29335=CARTESIAN_POINT('Ctrl Pts',(-1.4851881711891,-1.,-1.28435533880201));
#29336=CARTESIAN_POINT('Ctrl Pts',(-1.4851881711891,1.,-1.28435533880201));
#29337=CARTESIAN_POINT('Ctrl Pts',(-1.4906522831278,-1.,-1.2867467611644));
#29338=CARTESIAN_POINT('Ctrl Pts',(-1.4906522831278,1.,-1.2867467611644));
#29339=CARTESIAN_POINT('Ctrl Pts',(-1.49618896881754,-1.,-1.28911506584254));
#29340=CARTESIAN_POINT('Ctrl Pts',(-1.49618896881754,1.,-1.28911506584254));
#29341=CARTESIAN_POINT('Ctrl Pts',(-1.50178230149776,-1.,-1.29145022885181));
#29342=CARTESIAN_POINT('Ctrl Pts',(-1.50178230149776,1.,-1.29145022885181));
#29343=CARTESIAN_POINT('Ctrl Pts',(-1.50741159078365,-1.,-1.29373841372842));
#29344=CARTESIAN_POINT('Ctrl Pts',(-1.50741159078365,1.,-1.29373841372842));
#29345=CARTESIAN_POINT('Ctrl Pts',(-1.51305994241402,-1.,-1.29596850710509));
#29346=CARTESIAN_POINT('Ctrl Pts',(-1.51305994241402,1.,-1.29596850710509));
#29347=CARTESIAN_POINT('Ctrl Pts',(-1.51872184912724,-1.,-1.29813791800747));
#29348=CARTESIAN_POINT('Ctrl Pts',(-1.51872184912724,1.,-1.29813791800747));
#29349=CARTESIAN_POINT('Ctrl Pts',(-1.52439957861062,-1.,-1.30024984366328));
#29350=CARTESIAN_POINT('Ctrl Pts',(-1.52439957861062,1.,-1.30024984366328));
#29351=CARTESIAN_POINT('Ctrl Pts',(-1.53009970283891,-1.,-1.30231064395568));
#29352=CARTESIAN_POINT('Ctrl Pts',(-1.53009970283891,1.,-1.30231064395568));
#29353=CARTESIAN_POINT('Ctrl Pts',(-1.53582981268977,-1.,-1.30432735639489));
#29354=CARTESIAN_POINT('Ctrl Pts',(-1.53582981268977,1.,-1.30432735639489));
#29355=CARTESIAN_POINT('Ctrl Pts',(-1.54159462645432,-1.,-1.30630475189556));
#29356=CARTESIAN_POINT('Ctrl Pts',(-1.54159462645432,1.,-1.30630475189556));
#29357=CARTESIAN_POINT('Ctrl Pts',(-1.54739413957185,-1.,-1.30824393907473));
#29358=CARTESIAN_POINT('Ctrl Pts',(-1.54739413957185,1.,-1.30824393907473));
#29359=CARTESIAN_POINT('Ctrl Pts',(-1.55322568759481,-1.,-1.31014393684222));
#29360=CARTESIAN_POINT('Ctrl Pts',(-1.55322568759481,1.,-1.31014393684222));
#29361=CARTESIAN_POINT('Ctrl Pts',(-1.55908521254821,-1.,-1.31200264341696));
#29362=CARTESIAN_POINT('Ctrl Pts',(-1.55908521254821,1.,-1.31200264341696));
#29363=CARTESIAN_POINT('Ctrl Pts',(-1.56496872402353,-1.,-1.31381795281002));
#29364=CARTESIAN_POINT('Ctrl Pts',(-1.56496872402353,1.,-1.31381795281002));
#29365=CARTESIAN_POINT('Ctrl Pts',(-1.57087397835723,-1.,-1.31558903860016));
#29366=CARTESIAN_POINT('Ctrl Pts',(-1.57087397835723,1.,-1.31558903860016));
#29367=CARTESIAN_POINT('Ctrl Pts',(-1.5768005650559,-1.,-1.31731642317187));
#29368=CARTESIAN_POINT('Ctrl Pts',(-1.5768005650559,1.,-1.31731642317187));
#29369=CARTESIAN_POINT('Ctrl Pts',(-1.58274907898834,-1.,-1.31900135021432));
#29370=CARTESIAN_POINT('Ctrl Pts',(-1.58274907898834,1.,-1.31900135021432));
#29371=CARTESIAN_POINT('Ctrl Pts',(-1.58872057258245,-1.,-1.32064537110892));
#29372=CARTESIAN_POINT('Ctrl Pts',(-1.58872057258245,1.,-1.32064537110892));
#29373=CARTESIAN_POINT('Ctrl Pts',(-1.59471591079403,-1.,-1.32224985747682));
#29374=CARTESIAN_POINT('Ctrl Pts',(-1.59471591079403,1.,-1.32224985747682));
#29375=CARTESIAN_POINT('Ctrl Pts',(-1.60073511858687,-1.,-1.32381550858256));
#29376=CARTESIAN_POINT('Ctrl Pts',(-1.60073511858687,1.,-1.32381550858256));
#29377=CARTESIAN_POINT('Ctrl Pts',(-1.60677758290954,-1.,-1.32534250785782));
#29378=CARTESIAN_POINT('Ctrl Pts',(-1.60677758290954,1.,-1.32534250785782));
#29379=CARTESIAN_POINT('Ctrl Pts',(-1.6128423401575,-1.,-1.32683074483356));
#29380=CARTESIAN_POINT('Ctrl Pts',(-1.6128423401575,1.,-1.32683074483356));
#29381=CARTESIAN_POINT('Ctrl Pts',(-1.61892832270724,-1.,-1.32828000610449));
#29382=CARTESIAN_POINT('Ctrl Pts',(-1.61892832270724,1.,-1.32828000610449));
#29383=CARTESIAN_POINT('Ctrl Pts',(-1.62503464209797,-1.,-1.3296901950568));
#29384=CARTESIAN_POINT('Ctrl Pts',(-1.62503464209797,1.,-1.3296901950568));
#29385=CARTESIAN_POINT('Ctrl Pts',(-1.63116079730923,-1.,-1.33106149345645));
#29386=CARTESIAN_POINT('Ctrl Pts',(-1.63116079730923,1.,-1.33106149345645));
#29387=CARTESIAN_POINT('Ctrl Pts',(-1.63730653475089,-1.,-1.33239425103724));
#29388=CARTESIAN_POINT('Ctrl Pts',(-1.63730653475089,1.,-1.33239425103724));
#29389=CARTESIAN_POINT('Ctrl Pts',(-1.6434717485603,-1.,-1.33368890676572));
#29390=CARTESIAN_POINT('Ctrl Pts',(-1.6434717485603,1.,-1.33368890676572));
#29391=CARTESIAN_POINT('Ctrl Pts',(-1.6496563728683,-1.,-1.33494590467993));
#29392=CARTESIAN_POINT('Ctrl Pts',(-1.6496563728683,1.,-1.33494590467993));
#29393=CARTESIAN_POINT('Ctrl Pts',(-1.65586025952593,-1.,-1.33616559745172));
#29394=CARTESIAN_POINT('Ctrl Pts',(-1.65586025952593,1.,-1.33616559745172));
#29395=CARTESIAN_POINT('Ctrl Pts',(-1.66208312541983,-1.,-1.33734820885262));
#29396=CARTESIAN_POINT('Ctrl Pts',(-1.66208312541983,1.,-1.33734820885262));
#29397=CARTESIAN_POINT('Ctrl Pts',(-1.66832460783989,-1.,-1.33849388654388));
#29398=CARTESIAN_POINT('Ctrl Pts',(-1.66832460783989,1.,-1.33849388654388));
#29399=CARTESIAN_POINT('Ctrl Pts',(-1.67458429426086,-1.,-1.3396027347034));
#29400=CARTESIAN_POINT('Ctrl Pts',(-1.67458429426086,1.,-1.3396027347034));
#29401=CARTESIAN_POINT('Ctrl Pts',(-1.68086176030362,-1.,-1.34067485185203));
#29402=CARTESIAN_POINT('Ctrl Pts',(-1.68086176030362,1.,-1.34067485185203));
#29403=CARTESIAN_POINT('Ctrl Pts',(-1.68715660868764,-1.,-1.341710374848));
#29404=CARTESIAN_POINT('Ctrl Pts',(-1.68715660868764,1.,-1.341710374848));
#29405=CARTESIAN_POINT('Ctrl Pts',(-1.6934684849687,-1.,-1.34270948206319));
#29406=CARTESIAN_POINT('Ctrl Pts',(-1.6934684849687,1.,-1.34270948206319));
#29407=CARTESIAN_POINT('Ctrl Pts',(-1.69979707754427,-1.,-1.34367237124483));
#29408=CARTESIAN_POINT('Ctrl Pts',(-1.69979707754427,1.,-1.34367237124483));
#29409=CARTESIAN_POINT('Ctrl Pts',(-1.70614212266738,-1.,-1.34459924533831));
#29410=CARTESIAN_POINT('Ctrl Pts',(-1.70614212266738,1.,-1.34459924533831));
#29411=CARTESIAN_POINT('Ctrl Pts',(-1.71250340686822,-1.,-1.34549029589416));
#29412=CARTESIAN_POINT('Ctrl Pts',(-1.71250340686822,1.,-1.34549029589416));
#29413=CARTESIAN_POINT('Ctrl Pts',(-1.7188807715049,-1.,-1.34634568653227));
#29414=CARTESIAN_POINT('Ctrl Pts',(-1.7188807715049,1.,-1.34634568653227));
#29415=CARTESIAN_POINT('Ctrl Pts',(-1.72527410680674,-1.,-1.34716554819527));
#29416=CARTESIAN_POINT('Ctrl Pts',(-1.72527410680674,1.,-1.34716554819527));
#29417=CARTESIAN_POINT('Ctrl Pts',(-1.7304014965394,-1.,-1.34779309152035));
#29418=CARTESIAN_POINT('Ctrl Pts',(-1.7304014965394,1.,-1.34779309152035));
#29419=CARTESIAN_POINT('Ctrl Pts',(-1.73425417885907,-1.,-1.34824783112887));
#29420=CARTESIAN_POINT('Ctrl Pts',(-1.73425417885907,1.,-1.34824783112887));
#29421=CARTESIAN_POINT('Ctrl Pts',(-1.73682580585691,-1.,-1.34854391898045));
#29422=CARTESIAN_POINT('Ctrl Pts',(-1.73682580585691,1.,-1.34854391898045));
#29423=CARTESIAN_POINT('Ctrl Pts',(-1.73811241238545,-1.,-1.34869019493419));
#29424=CARTESIAN_POINT('Ctrl Pts',(-1.73811241238545,1.,-1.34869019493419));
#29425=CARTESIAN_POINT('',(-1.31362392696032,1.,-1.15624053661742));
#29426=CARTESIAN_POINT('Ctrl Pts',(-1.31362392696032,1.,-1.15624053661742));
#29427=CARTESIAN_POINT('Ctrl Pts',(-1.31722977216397,1.,-1.15950888730809));
#29428=CARTESIAN_POINT('Ctrl Pts',(-1.32428080721772,1.,-1.16589330093588));
#29429=CARTESIAN_POINT('Ctrl Pts',(-1.33437539347008,1.,-1.17501305789857));
#29430=CARTESIAN_POINT('Ctrl Pts',(-1.34687054001093,1.,-1.18625865667441));
#29431=CARTESIAN_POINT('Ctrl Pts',(-1.36088705043885,1.,-1.1987959077932));
#29432=CARTESIAN_POINT('Ctrl Pts',(-1.37331915607905,1.,-1.20982812925645));
#29433=CARTESIAN_POINT('Ctrl Pts',(-1.38420564527715,1.,-1.21938737280852));
#29434=CARTESIAN_POINT('Ctrl Pts',(-1.39361389568796,1.,-1.22752961899387));
#29435=CARTESIAN_POINT('Ctrl Pts',(-1.40164708206106,1.,-1.23434087290423));
#29436=CARTESIAN_POINT('Ctrl Pts',(-1.40845295531283,1.,-1.23994455029534));
#29437=CARTESIAN_POINT('Ctrl Pts',(-1.41422913175179,1.,-1.24450600513056));
#29438=CARTESIAN_POINT('Ctrl Pts',(-1.41923722596025,1.,-1.24824430986571));
#29439=CARTESIAN_POINT('Ctrl Pts',(-1.42378102115575,1.,-1.2514145557001));
#29440=CARTESIAN_POINT('Ctrl Pts',(-1.42815938799387,1.,-1.25426945222639));
#29441=CARTESIAN_POINT('Ctrl Pts',(-1.43262645609691,1.,-1.25702687965755));
#29442=CARTESIAN_POINT('Ctrl Pts',(-1.43734919180848,1.,-1.25983531012005));
#29443=CARTESIAN_POINT('Ctrl Pts',(-1.44236470511303,1.,-1.26273903323859));
#29444=CARTESIAN_POINT('Ctrl Pts',(-1.44761985001662,1.,-1.26570925118868));
#29445=CARTESIAN_POINT('Ctrl Pts',(-1.45301422764247,1.,-1.2686778680489));
#29446=CARTESIAN_POINT('Ctrl Pts',(-1.45843906294697,1.,-1.27156805265289));
#29447=CARTESIAN_POINT('Ctrl Pts',(-1.46382431332476,1.,-1.27433119897822));
#29448=CARTESIAN_POINT('Ctrl Pts',(-1.46916035917133,1.,-1.27696414831089));
#29449=CARTESIAN_POINT('Ctrl Pts',(-1.4744717526707,1.,-1.2794891824849));
#29450=CARTESIAN_POINT('Ctrl Pts',(-1.47980070347095,1.,-1.28194158939517));
#29451=CARTESIAN_POINT('Ctrl Pts',(-1.4851881711891,1.,-1.28435533880201));
#29452=CARTESIAN_POINT('Ctrl Pts',(-1.4906522831278,1.,-1.2867467611644));
#29453=CARTESIAN_POINT('Ctrl Pts',(-1.49618896881754,1.,-1.28911506584254));
#29454=CARTESIAN_POINT('Ctrl Pts',(-1.50178230149776,1.,-1.29145022885181));
#29455=CARTESIAN_POINT('Ctrl Pts',(-1.50741159078365,1.,-1.29373841372842));
#29456=CARTESIAN_POINT('Ctrl Pts',(-1.51305994241402,1.,-1.29596850710509));
#29457=CARTESIAN_POINT('Ctrl Pts',(-1.51872184912724,1.,-1.29813791800747));
#29458=CARTESIAN_POINT('Ctrl Pts',(-1.52439957861062,1.,-1.30024984366328));
#29459=CARTESIAN_POINT('Ctrl Pts',(-1.53009970283891,1.,-1.30231064395568));
#29460=CARTESIAN_POINT('Ctrl Pts',(-1.53582981268977,1.,-1.30432735639489));
#29461=CARTESIAN_POINT('Ctrl Pts',(-1.54159462645432,1.,-1.30630475189556));
#29462=CARTESIAN_POINT('Ctrl Pts',(-1.54739413957185,1.,-1.30824393907473));
#29463=CARTESIAN_POINT('Ctrl Pts',(-1.55322568759481,1.,-1.31014393684222));
#29464=CARTESIAN_POINT('Ctrl Pts',(-1.55908521254821,1.,-1.31200264341696));
#29465=CARTESIAN_POINT('Ctrl Pts',(-1.56496872402353,1.,-1.31381795281002));
#29466=CARTESIAN_POINT('Ctrl Pts',(-1.57087397835723,1.,-1.31558903860016));
#29467=CARTESIAN_POINT('Ctrl Pts',(-1.5768005650559,1.,-1.31731642317187));
#29468=CARTESIAN_POINT('Ctrl Pts',(-1.58274907898834,1.,-1.31900135021432));
#29469=CARTESIAN_POINT('Ctrl Pts',(-1.58872057258245,1.,-1.32064537110892));
#29470=CARTESIAN_POINT('Ctrl Pts',(-1.59471591079403,1.,-1.32224985747682));
#29471=CARTESIAN_POINT('Ctrl Pts',(-1.60073511858687,1.,-1.32381550858256));
#29472=CARTESIAN_POINT('Ctrl Pts',(-1.60677758290954,1.,-1.32534250785782));
#29473=CARTESIAN_POINT('Ctrl Pts',(-1.6128423401575,1.,-1.32683074483356));
#29474=CARTESIAN_POINT('Ctrl Pts',(-1.61892832270724,1.,-1.32828000610449));
#29475=CARTESIAN_POINT('Ctrl Pts',(-1.62503464209797,1.,-1.3296901950568));
#29476=CARTESIAN_POINT('Ctrl Pts',(-1.63116079730923,1.,-1.33106149345645));
#29477=CARTESIAN_POINT('Ctrl Pts',(-1.63730653475089,1.,-1.33239425103724));
#29478=CARTESIAN_POINT('Ctrl Pts',(-1.6434717485603,1.,-1.33368890676572));
#29479=CARTESIAN_POINT('Ctrl Pts',(-1.6496563728683,1.,-1.33494590467993));
#29480=CARTESIAN_POINT('Ctrl Pts',(-1.65586025952593,1.,-1.33616559745172));
#29481=CARTESIAN_POINT('Ctrl Pts',(-1.66208312541983,1.,-1.33734820885262));
#29482=CARTESIAN_POINT('Ctrl Pts',(-1.66832460783989,1.,-1.33849388654388));
#29483=CARTESIAN_POINT('Ctrl Pts',(-1.67458429426086,1.,-1.3396027347034));
#29484=CARTESIAN_POINT('Ctrl Pts',(-1.68086176030362,1.,-1.34067485185203));
#29485=CARTESIAN_POINT('Ctrl Pts',(-1.68715660868764,1.,-1.341710374848));
#29486=CARTESIAN_POINT('Ctrl Pts',(-1.6934684849687,1.,-1.34270948206319));
#29487=CARTESIAN_POINT('Ctrl Pts',(-1.69979707754427,1.,-1.34367237124483));
#29488=CARTESIAN_POINT('Ctrl Pts',(-1.70614212266738,1.,-1.34459924533831));
#29489=CARTESIAN_POINT('Ctrl Pts',(-1.71250340686822,1.,-1.34549029589416));
#29490=CARTESIAN_POINT('Ctrl Pts',(-1.7188807715049,1.,-1.34634568653227));
#29491=CARTESIAN_POINT('Ctrl Pts',(-1.72527410680674,1.,-1.34716554819527));
#29492=CARTESIAN_POINT('Ctrl Pts',(-1.7304014965394,1.,-1.34779309152035));
#29493=CARTESIAN_POINT('Ctrl Pts',(-1.73425417885907,1.,-1.34824783112887));
#29494=CARTESIAN_POINT('Ctrl Pts',(-1.73682580585691,1.,-1.34854391898045));
#29495=CARTESIAN_POINT('Ctrl Pts',(-1.73811241238545,1.,-1.34869019493419));
#29496=CARTESIAN_POINT('',(-1.31362392696032,0.,-1.15624053661742));
#29497=CARTESIAN_POINT('Origin',(0.,0.,0.));
#29498=CARTESIAN_POINT('',(-1.15624053661742,1.,-1.31362392696033));
#29499=CARTESIAN_POINT('Origin',(0.,1.,0.));
#29500=CARTESIAN_POINT('',(-1.15624053661742,0.,-1.31362392696033));
#29501=CARTESIAN_POINT('Ctrl Pts',(-1.34869019493419,-1.,-1.73811241238545));
#29502=CARTESIAN_POINT('Ctrl Pts',(-1.34869019493419,1.,-1.73811241238545));
#29503=CARTESIAN_POINT('Ctrl Pts',(-1.34854391898145,-1.,-1.73682580585819));
#29504=CARTESIAN_POINT('Ctrl Pts',(-1.34854391898145,1.,-1.73682580585819));
#29505=CARTESIAN_POINT('Ctrl Pts',(-1.34824783113158,-1.,-1.73425417886255));
#29506=CARTESIAN_POINT('Ctrl Pts',(-1.34824783113158,1.,-1.73425417886255));
#29507=CARTESIAN_POINT('Ctrl Pts',(-1.3477930915247,-1.,-1.73040149654497));
#29508=CARTESIAN_POINT('Ctrl Pts',(-1.3477930915247,1.,-1.73040149654497));
#29509=CARTESIAN_POINT('Ctrl Pts',(-1.34716554820013,-1.,-1.72527410681298));
#29510=CARTESIAN_POINT('Ctrl Pts',(-1.34716554820013,1.,-1.72527410681298));
#29511=CARTESIAN_POINT('Ctrl Pts',(-1.34634568653586,-1.,-1.7188807715095));
#29512=CARTESIAN_POINT('Ctrl Pts',(-1.34634568653586,1.,-1.7188807715095));
#29513=CARTESIAN_POINT('Ctrl Pts',(-1.34549029589563,-1.,-1.71250340687011));
#29514=CARTESIAN_POINT('Ctrl Pts',(-1.34549029589563,1.,-1.71250340687011));
#29515=CARTESIAN_POINT('Ctrl Pts',(-1.34459924533783,-1.,-1.70614212266676));
#29516=CARTESIAN_POINT('Ctrl Pts',(-1.34459924533783,1.,-1.70614212266676));
#29517=CARTESIAN_POINT('Ctrl Pts',(-1.34367237124322,-1.,-1.69979707754221));
#29518=CARTESIAN_POINT('Ctrl Pts',(-1.34367237124322,1.,-1.69979707754221));
#29519=CARTESIAN_POINT('Ctrl Pts',(-1.34270948206139,-1.,-1.6934684849664));
#29520=CARTESIAN_POINT('Ctrl Pts',(-1.34270948206139,1.,-1.6934684849664));
#29521=CARTESIAN_POINT('Ctrl Pts',(-1.34171037484673,-1.,-1.68715660868602));
#29522=CARTESIAN_POINT('Ctrl Pts',(-1.34171037484673,1.,-1.68715660868602));
#29523=CARTESIAN_POINT('Ctrl Pts',(-1.3406748518516,-1.,-1.68086176030308));
#29524=CARTESIAN_POINT('Ctrl Pts',(-1.3406748518516,1.,-1.68086176030308));
#29525=CARTESIAN_POINT('Ctrl Pts',(-1.33960273470372,-1.,-1.67458429426126));
#29526=CARTESIAN_POINT('Ctrl Pts',(-1.33960273470372,1.,-1.67458429426126));
#29527=CARTESIAN_POINT('Ctrl Pts',(-1.33849388654458,-1.,-1.66832460784078));
#29528=CARTESIAN_POINT('Ctrl Pts',(-1.33849388654458,1.,-1.66832460784078));
#29529=CARTESIAN_POINT('Ctrl Pts',(-1.33734820885331,-1.,-1.66208312542073));
#29530=CARTESIAN_POINT('Ctrl Pts',(-1.33734820885331,1.,-1.66208312542073));
#29531=CARTESIAN_POINT('Ctrl Pts',(-1.33616559745217,-1.,-1.65586025952651));
#29532=CARTESIAN_POINT('Ctrl Pts',(-1.33616559745217,1.,-1.65586025952651));
#29533=CARTESIAN_POINT('Ctrl Pts',(-1.33494590468003,-1.,-1.64965637286843));
#29534=CARTESIAN_POINT('Ctrl Pts',(-1.33494590468003,1.,-1.64965637286843));
#29535=CARTESIAN_POINT('Ctrl Pts',(-1.33368890676554,-1.,-1.64347174856007));
#29536=CARTESIAN_POINT('Ctrl Pts',(-1.33368890676554,1.,-1.64347174856007));
#29537=CARTESIAN_POINT('Ctrl Pts',(-1.33239425103694,-1.,-1.6373065347505));
#29538=CARTESIAN_POINT('Ctrl Pts',(-1.33239425103694,1.,-1.6373065347505));
#29539=CARTESIAN_POINT('Ctrl Pts',(-1.33106149345618,-1.,-1.63116079730887));
#29540=CARTESIAN_POINT('Ctrl Pts',(-1.33106149345618,1.,-1.63116079730887));
#29541=CARTESIAN_POINT('Ctrl Pts',(-1.32969019505665,-1.,-1.62503464209777));
#29542=CARTESIAN_POINT('Ctrl Pts',(-1.32969019505665,1.,-1.62503464209777));
#29543=CARTESIAN_POINT('Ctrl Pts',(-1.32828000610448,-1.,-1.61892832270723));
#29544=CARTESIAN_POINT('Ctrl Pts',(-1.32828000610448,1.,-1.61892832270723));
#29545=CARTESIAN_POINT('Ctrl Pts',(-1.32683074483365,-1.,-1.61284234015762));
#29546=CARTESIAN_POINT('Ctrl Pts',(-1.32683074483365,1.,-1.61284234015762));
#29547=CARTESIAN_POINT('Ctrl Pts',(-1.32534250785794,-1.,-1.6067775829097));
#29548=CARTESIAN_POINT('Ctrl Pts',(-1.32534250785794,1.,-1.6067775829097));
#29549=CARTESIAN_POINT('Ctrl Pts',(-1.32381550858266,-1.,-1.600735118587));
#29550=CARTESIAN_POINT('Ctrl Pts',(-1.32381550858266,1.,-1.600735118587));
#29551=CARTESIAN_POINT('Ctrl Pts',(-1.32224985747686,-1.,-1.59471591079408));
#29552=CARTESIAN_POINT('Ctrl Pts',(-1.32224985747686,1.,-1.59471591079408));
#29553=CARTESIAN_POINT('Ctrl Pts',(-1.32064537110891,-1.,-1.58872057258244));
#29554=CARTESIAN_POINT('Ctrl Pts',(-1.32064537110891,1.,-1.58872057258244));
#29555=CARTESIAN_POINT('Ctrl Pts',(-1.31900135021428,-1.,-1.58274907898829));
#29556=CARTESIAN_POINT('Ctrl Pts',(-1.31900135021428,1.,-1.58274907898829));
#29557=CARTESIAN_POINT('Ctrl Pts',(-1.31731642317183,-1.,-1.57680056505585));
#29558=CARTESIAN_POINT('Ctrl Pts',(-1.31731642317183,1.,-1.57680056505585));
#29559=CARTESIAN_POINT('Ctrl Pts',(-1.31558903860015,-1.,-1.57087397835721));
#29560=CARTESIAN_POINT('Ctrl Pts',(-1.31558903860015,1.,-1.57087397835721));
#29561=CARTESIAN_POINT('Ctrl Pts',(-1.31381795281002,-1.,-1.56496872402352));
#29562=CARTESIAN_POINT('Ctrl Pts',(-1.31381795281002,1.,-1.56496872402352));
#29563=CARTESIAN_POINT('Ctrl Pts',(-1.31200264341696,-1.,-1.55908521254822));
#29564=CARTESIAN_POINT('Ctrl Pts',(-1.31200264341696,1.,-1.55908521254822));
#29565=CARTESIAN_POINT('Ctrl Pts',(-1.31014393684221,-1.,-1.55322568759481));
#29566=CARTESIAN_POINT('Ctrl Pts',(-1.31014393684221,1.,-1.55322568759481));
#29567=CARTESIAN_POINT('Ctrl Pts',(-1.30824393907471,-1.,-1.54739413957183));
#29568=CARTESIAN_POINT('Ctrl Pts',(-1.30824393907471,1.,-1.54739413957183));
#29569=CARTESIAN_POINT('Ctrl Pts',(-1.30630475189553,-1.,-1.54159462645428));
#29570=CARTESIAN_POINT('Ctrl Pts',(-1.30630475189553,1.,-1.54159462645428));
#29571=CARTESIAN_POINT('Ctrl Pts',(-1.30432735639487,-1.,-1.53582981268976));
#29572=CARTESIAN_POINT('Ctrl Pts',(-1.30432735639487,1.,-1.53582981268976));
#29573=CARTESIAN_POINT('Ctrl Pts',(-1.3023106439557,-1.,-1.53009970283893));
#29574=CARTESIAN_POINT('Ctrl Pts',(-1.3023106439557,1.,-1.53009970283893));
#29575=CARTESIAN_POINT('Ctrl Pts',(-1.30024984366334,-1.,-1.5243995786107));
#29576=CARTESIAN_POINT('Ctrl Pts',(-1.30024984366334,1.,-1.5243995786107));
#29577=CARTESIAN_POINT('Ctrl Pts',(-1.29813791800757,-1.,-1.51872184912735));
#29578=CARTESIAN_POINT('Ctrl Pts',(-1.29813791800757,1.,-1.51872184912735));
#29579=CARTESIAN_POINT('Ctrl Pts',(-1.29596850710518,-1.,-1.51305994241412));
#29580=CARTESIAN_POINT('Ctrl Pts',(-1.29596850710518,1.,-1.51305994241412));
#29581=CARTESIAN_POINT('Ctrl Pts',(-1.29373841372843,-1.,-1.50741159078367));
#29582=CARTESIAN_POINT('Ctrl Pts',(-1.29373841372843,1.,-1.50741159078367));
#29583=CARTESIAN_POINT('Ctrl Pts',(-1.29145022885171,-1.,-1.50178230149764));
#29584=CARTESIAN_POINT('Ctrl Pts',(-1.29145022885171,1.,-1.50178230149764));
#29585=CARTESIAN_POINT('Ctrl Pts',(-1.28911506584232,-1.,-1.49618896881729));
#29586=CARTESIAN_POINT('Ctrl Pts',(-1.28911506584232,1.,-1.49618896881729));
#29587=CARTESIAN_POINT('Ctrl Pts',(-1.28674676116415,-1.,-1.4906522831275));
#29588=CARTESIAN_POINT('Ctrl Pts',(-1.28674676116415,1.,-1.4906522831275));
#29589=CARTESIAN_POINT('Ctrl Pts',(-1.28435533880184,-1.,-1.48518817118891));
#29590=CARTESIAN_POINT('Ctrl Pts',(-1.28435533880184,1.,-1.48518817118891));
#29591=CARTESIAN_POINT('Ctrl Pts',(-1.28194158939522,-1.,-1.47980070347102));
#29592=CARTESIAN_POINT('Ctrl Pts',(-1.28194158939522,1.,-1.47980070347102));
#29593=CARTESIAN_POINT('Ctrl Pts',(-1.27948918248524,-1.,-1.4744717526711));
#29594=CARTESIAN_POINT('Ctrl Pts',(-1.27948918248524,1.,-1.4744717526711));
#29595=CARTESIAN_POINT('Ctrl Pts',(-1.27696414831144,-1.,-1.46916035917197));
#29596=CARTESIAN_POINT('Ctrl Pts',(-1.27696414831144,1.,-1.46916035917197));
#29597=CARTESIAN_POINT('Ctrl Pts',(-1.27433119897877,-1.,-1.4638243133254));
#29598=CARTESIAN_POINT('Ctrl Pts',(-1.27433119897877,1.,-1.4638243133254));
#29599=CARTESIAN_POINT('Ctrl Pts',(-1.27156805265312,-1.,-1.45843906294725));
#29600=CARTESIAN_POINT('Ctrl Pts',(-1.27156805265312,1.,-1.45843906294725));
#29601=CARTESIAN_POINT('Ctrl Pts',(-1.26867786804854,-1.,-1.45301422764205));
#29602=CARTESIAN_POINT('Ctrl Pts',(-1.26867786804854,1.,-1.45301422764205));
#29603=CARTESIAN_POINT('Ctrl Pts',(-1.26570925118767,-1.,-1.44761985001544));
#29604=CARTESIAN_POINT('Ctrl Pts',(-1.26570925118767,1.,-1.44761985001544));
#29605=CARTESIAN_POINT('Ctrl Pts',(-1.26273903323723,-1.,-1.44236470511145));
#29606=CARTESIAN_POINT('Ctrl Pts',(-1.26273903323723,1.,-1.44236470511145));
#29607=CARTESIAN_POINT('Ctrl Pts',(-1.25983531011894,-1.,-1.43734919180719));
#29608=CARTESIAN_POINT('Ctrl Pts',(-1.25983531011894,1.,-1.43734919180719));
#29609=CARTESIAN_POINT('Ctrl Pts',(-1.25702687965744,-1.,-1.43262645609679));
#29610=CARTESIAN_POINT('Ctrl Pts',(-1.25702687965744,1.,-1.43262645609679));
#29611=CARTESIAN_POINT('Ctrl Pts',(-1.25426945222783,-1.,-1.42815938799555));
#29612=CARTESIAN_POINT('Ctrl Pts',(-1.25426945222783,1.,-1.42815938799555));
#29613=CARTESIAN_POINT('Ctrl Pts',(-1.25141455570299,-1.,-1.42378102115911));
#29614=CARTESIAN_POINT('Ctrl Pts',(-1.25141455570299,1.,-1.42378102115911));
#29615=CARTESIAN_POINT('Ctrl Pts',(-1.24824430986911,-1.,-1.41923722596421));
#29616=CARTESIAN_POINT('Ctrl Pts',(-1.24824430986911,1.,-1.41923722596421));
#29617=CARTESIAN_POINT('Ctrl Pts',(-1.24450600513278,-1.,-1.41422913175437));
#29618=CARTESIAN_POINT('Ctrl Pts',(-1.24450600513278,1.,-1.41422913175437));
#29619=CARTESIAN_POINT('Ctrl Pts',(-1.23994455029421,-1.,-1.40845295531151));
#29620=CARTESIAN_POINT('Ctrl Pts',(-1.23994455029421,1.,-1.40845295531151));
#29621=CARTESIAN_POINT('Ctrl Pts',(-1.23434087289768,-1.,-1.40164708205345));
#29622=CARTESIAN_POINT('Ctrl Pts',(-1.23434087289768,1.,-1.40164708205345));
#29623=CARTESIAN_POINT('Ctrl Pts',(-1.22752961898063,-1.,-1.39361389567257));
#29624=CARTESIAN_POINT('Ctrl Pts',(-1.22752961898063,1.,-1.39361389567257));
#29625=CARTESIAN_POINT('Ctrl Pts',(-1.21938737278853,-1.,-1.38420564525391));
#29626=CARTESIAN_POINT('Ctrl Pts',(-1.21938737278853,1.,-1.38420564525391));
#29627=CARTESIAN_POINT('Ctrl Pts',(-1.20982812923113,-1.,-1.37331915604962));
#29628=CARTESIAN_POINT('Ctrl Pts',(-1.20982812923113,1.,-1.37331915604962));
#29629=CARTESIAN_POINT('Ctrl Pts',(-1.1987959077656,-1.,-1.36088705040677));
#29630=CARTESIAN_POINT('Ctrl Pts',(-1.1987959077656,1.,-1.36088705040677));
#29631=CARTESIAN_POINT('Ctrl Pts',(-1.18625865664915,-1.,-1.34687053998157));
#29632=CARTESIAN_POINT('Ctrl Pts',(-1.18625865664915,1.,-1.34687053998157));
#29633=CARTESIAN_POINT('Ctrl Pts',(-1.17501305787994,-1.,-1.33437539344842));
#29634=CARTESIAN_POINT('Ctrl Pts',(-1.17501305787994,1.,-1.33437539344842));
#29635=CARTESIAN_POINT('Ctrl Pts',(-1.16589330092532,-1.,-1.32428080720544));
#29636=CARTESIAN_POINT('Ctrl Pts',(-1.16589330092532,1.,-1.32428080720544));
#29637=CARTESIAN_POINT('Ctrl Pts',(-1.15950888730433,-1.,-1.3172297721596));
#29638=CARTESIAN_POINT('Ctrl Pts',(-1.15950888730433,1.,-1.3172297721596));
#29639=CARTESIAN_POINT('Ctrl Pts',(-1.15624053661742,-1.,-1.31362392696033));
#29640=CARTESIAN_POINT('Ctrl Pts',(-1.15624053661742,1.,-1.31362392696033));
#29641=CARTESIAN_POINT('',(-1.34869019493419,1.,-1.73811241238545));
#29642=CARTESIAN_POINT('Ctrl Pts',(-1.34869019493419,1.,-1.73811241238545));
#29643=CARTESIAN_POINT('Ctrl Pts',(-1.34854391898145,1.,-1.73682580585819));
#29644=CARTESIAN_POINT('Ctrl Pts',(-1.34824783113158,1.,-1.73425417886255));
#29645=CARTESIAN_POINT('Ctrl Pts',(-1.3477930915247,1.,-1.73040149654497));
#29646=CARTESIAN_POINT('Ctrl Pts',(-1.34716554820013,1.,-1.72527410681298));
#29647=CARTESIAN_POINT('Ctrl Pts',(-1.34634568653586,1.,-1.7188807715095));
#29648=CARTESIAN_POINT('Ctrl Pts',(-1.34549029589563,1.,-1.71250340687011));
#29649=CARTESIAN_POINT('Ctrl Pts',(-1.34459924533783,1.,-1.70614212266676));
#29650=CARTESIAN_POINT('Ctrl Pts',(-1.34367237124322,1.,-1.69979707754221));
#29651=CARTESIAN_POINT('Ctrl Pts',(-1.34270948206139,1.,-1.6934684849664));
#29652=CARTESIAN_POINT('Ctrl Pts',(-1.34171037484673,1.,-1.68715660868602));
#29653=CARTESIAN_POINT('Ctrl Pts',(-1.3406748518516,1.,-1.68086176030308));
#29654=CARTESIAN_POINT('Ctrl Pts',(-1.33960273470372,1.,-1.67458429426126));
#29655=CARTESIAN_POINT('Ctrl Pts',(-1.33849388654458,1.,-1.66832460784078));
#29656=CARTESIAN_POINT('Ctrl Pts',(-1.33734820885331,1.,-1.66208312542073));
#29657=CARTESIAN_POINT('Ctrl Pts',(-1.33616559745217,1.,-1.65586025952651));
#29658=CARTESIAN_POINT('Ctrl Pts',(-1.33494590468003,1.,-1.64965637286843));
#29659=CARTESIAN_POINT('Ctrl Pts',(-1.33368890676554,1.,-1.64347174856007));
#29660=CARTESIAN_POINT('Ctrl Pts',(-1.33239425103694,1.,-1.6373065347505));
#29661=CARTESIAN_POINT('Ctrl Pts',(-1.33106149345618,1.,-1.63116079730887));
#29662=CARTESIAN_POINT('Ctrl Pts',(-1.32969019505665,1.,-1.62503464209777));
#29663=CARTESIAN_POINT('Ctrl Pts',(-1.32828000610448,1.,-1.61892832270723));
#29664=CARTESIAN_POINT('Ctrl Pts',(-1.32683074483365,1.,-1.61284234015762));
#29665=CARTESIAN_POINT('Ctrl Pts',(-1.32534250785794,1.,-1.6067775829097));
#29666=CARTESIAN_POINT('Ctrl Pts',(-1.32381550858266,1.,-1.600735118587));
#29667=CARTESIAN_POINT('Ctrl Pts',(-1.32224985747686,1.,-1.59471591079408));
#29668=CARTESIAN_POINT('Ctrl Pts',(-1.32064537110891,1.,-1.58872057258244));
#29669=CARTESIAN_POINT('Ctrl Pts',(-1.31900135021428,1.,-1.58274907898829));
#29670=CARTESIAN_POINT('Ctrl Pts',(-1.31731642317183,1.,-1.57680056505585));
#29671=CARTESIAN_POINT('Ctrl Pts',(-1.31558903860015,1.,-1.57087397835721));
#29672=CARTESIAN_POINT('Ctrl Pts',(-1.31381795281002,1.,-1.56496872402352));
#29673=CARTESIAN_POINT('Ctrl Pts',(-1.31200264341696,1.,-1.55908521254822));
#29674=CARTESIAN_POINT('Ctrl Pts',(-1.31014393684221,1.,-1.55322568759481));
#29675=CARTESIAN_POINT('Ctrl Pts',(-1.30824393907471,1.,-1.54739413957183));
#29676=CARTESIAN_POINT('Ctrl Pts',(-1.30630475189553,1.,-1.54159462645428));
#29677=CARTESIAN_POINT('Ctrl Pts',(-1.30432735639487,1.,-1.53582981268976));
#29678=CARTESIAN_POINT('Ctrl Pts',(-1.3023106439557,1.,-1.53009970283893));
#29679=CARTESIAN_POINT('Ctrl Pts',(-1.30024984366334,1.,-1.5243995786107));
#29680=CARTESIAN_POINT('Ctrl Pts',(-1.29813791800757,1.,-1.51872184912735));
#29681=CARTESIAN_POINT('Ctrl Pts',(-1.29596850710518,1.,-1.51305994241412));
#29682=CARTESIAN_POINT('Ctrl Pts',(-1.29373841372843,1.,-1.50741159078367));
#29683=CARTESIAN_POINT('Ctrl Pts',(-1.29145022885171,1.,-1.50178230149764));
#29684=CARTESIAN_POINT('Ctrl Pts',(-1.28911506584232,1.,-1.49618896881729));
#29685=CARTESIAN_POINT('Ctrl Pts',(-1.28674676116415,1.,-1.4906522831275));
#29686=CARTESIAN_POINT('Ctrl Pts',(-1.28435533880184,1.,-1.48518817118891));
#29687=CARTESIAN_POINT('Ctrl Pts',(-1.28194158939522,1.,-1.47980070347102));
#29688=CARTESIAN_POINT('Ctrl Pts',(-1.27948918248524,1.,-1.4744717526711));
#29689=CARTESIAN_POINT('Ctrl Pts',(-1.27696414831144,1.,-1.46916035917197));
#29690=CARTESIAN_POINT('Ctrl Pts',(-1.27433119897877,1.,-1.4638243133254));
#29691=CARTESIAN_POINT('Ctrl Pts',(-1.27156805265312,1.,-1.45843906294725));
#29692=CARTESIAN_POINT('Ctrl Pts',(-1.26867786804854,1.,-1.45301422764205));
#29693=CARTESIAN_POINT('Ctrl Pts',(-1.26570925118767,1.,-1.44761985001544));
#29694=CARTESIAN_POINT('Ctrl Pts',(-1.26273903323723,1.,-1.44236470511145));
#29695=CARTESIAN_POINT('Ctrl Pts',(-1.25983531011894,1.,-1.43734919180719));
#29696=CARTESIAN_POINT('Ctrl Pts',(-1.25702687965744,1.,-1.43262645609679));
#29697=CARTESIAN_POINT('Ctrl Pts',(-1.25426945222783,1.,-1.42815938799555));
#29698=CARTESIAN_POINT('Ctrl Pts',(-1.25141455570299,1.,-1.42378102115911));
#29699=CARTESIAN_POINT('Ctrl Pts',(-1.24824430986911,1.,-1.41923722596421));
#29700=CARTESIAN_POINT('Ctrl Pts',(-1.24450600513278,1.,-1.41422913175437));
#29701=CARTESIAN_POINT('Ctrl Pts',(-1.23994455029421,1.,-1.40845295531151));
#29702=CARTESIAN_POINT('Ctrl Pts',(-1.23434087289768,1.,-1.40164708205345));
#29703=CARTESIAN_POINT('Ctrl Pts',(-1.22752961898063,1.,-1.39361389567257));
#29704=CARTESIAN_POINT('Ctrl Pts',(-1.21938737278853,1.,-1.38420564525391));
#29705=CARTESIAN_POINT('Ctrl Pts',(-1.20982812923113,1.,-1.37331915604962));
#29706=CARTESIAN_POINT('Ctrl Pts',(-1.1987959077656,1.,-1.36088705040677));
#29707=CARTESIAN_POINT('Ctrl Pts',(-1.18625865664915,1.,-1.34687053998157));
#29708=CARTESIAN_POINT('Ctrl Pts',(-1.17501305787994,1.,-1.33437539344842));
#29709=CARTESIAN_POINT('Ctrl Pts',(-1.16589330092532,1.,-1.32428080720544));
#29710=CARTESIAN_POINT('Ctrl Pts',(-1.15950888730433,1.,-1.3172297721596));
#29711=CARTESIAN_POINT('Ctrl Pts',(-1.15624053661742,1.,-1.31362392696033));
#29712=CARTESIAN_POINT('',(-1.34869019493419,0.,-1.73811241238545));
#29713=CARTESIAN_POINT('Origin',(-1.23627494547115,0.,-1.81978687191668));
#29714=CARTESIAN_POINT('',(-1.23627494547115,1.,-1.81978687191668));
#29715=CARTESIAN_POINT('',(-1.34869019493419,1.,-1.73811241238545));
#29716=CARTESIAN_POINT('',(-1.23627494547115,0.,-1.81978687191668));
#29717=CARTESIAN_POINT('Ctrl Pts',(-0.892032620296855,-1.,-1.5055822144029));
#29718=CARTESIAN_POINT('Ctrl Pts',(-0.892032620296855,1.,-1.5055822144029));
#29719=CARTESIAN_POINT('Ctrl Pts',(-0.894452006967538,-1.,-1.50980486807181));
#29720=CARTESIAN_POINT('Ctrl Pts',(-0.894452006967538,1.,-1.50980486807181));
#29721=CARTESIAN_POINT('Ctrl Pts',(-0.89918504749193,-1.,-1.51805569591479));
#29722=CARTESIAN_POINT('Ctrl Pts',(-0.89918504749193,1.,-1.51805569591479));
#29723=CARTESIAN_POINT('Ctrl Pts',(-0.905967409640499,-1.,-1.52984849890434));
#29724=CARTESIAN_POINT('Ctrl Pts',(-0.905967409640499,1.,-1.52984849890434));
#29725=CARTESIAN_POINT('Ctrl Pts',(-0.91437591904658,-1.,-1.54440491152808));
#29726=CARTESIAN_POINT('Ctrl Pts',(-0.91437591904658,1.,-1.54440491152808));
#29727=CARTESIAN_POINT('Ctrl Pts',(-0.923832188966322,-1.,-1.56065988582509));
#29728=CARTESIAN_POINT('Ctrl Pts',(-0.923832188966322,1.,-1.56065988582509));
#29729=CARTESIAN_POINT('Ctrl Pts',(-0.932246680128849,-1.,-1.57499388385561));
#29730=CARTESIAN_POINT('Ctrl Pts',(-0.932246680128849,1.,-1.57499388385561));
#29731=CARTESIAN_POINT('Ctrl Pts',(-0.939646377909319,-1.,-1.58744937489796));
#29732=CARTESIAN_POINT('Ctrl Pts',(-0.939646377909319,1.,-1.58744937489796));
#29733=CARTESIAN_POINT('Ctrl Pts',(-0.946078063325796,-1.,-1.59810042045408));
#29734=CARTESIAN_POINT('Ctrl Pts',(-0.946078063325796,1.,-1.59810042045408));
#29735=CARTESIAN_POINT('Ctrl Pts',(-0.951613284361248,-1.,-1.60706069897794));
#29736=CARTESIAN_POINT('Ctrl Pts',(-0.951613284361248,1.,-1.60706069897794));
#29737=CARTESIAN_POINT('Ctrl Pts',(-0.956354422921573,-1.,-1.61449324337233));
#29738=CARTESIAN_POINT('Ctrl Pts',(-0.956354422921573,1.,-1.61449324337233));
#29739=CARTESIAN_POINT('Ctrl Pts',(-0.960438326099958,-1.,-1.62061638139929));
#29740=CARTESIAN_POINT('Ctrl Pts',(-0.960438326099958,1.,-1.62061638139929));
#29741=CARTESIAN_POINT('Ctrl Pts',(-0.964046107037821,-1.,-1.6257193066974));
#29742=CARTESIAN_POINT('Ctrl Pts',(-0.964046107037821,1.,-1.6257193066974));
#29743=CARTESIAN_POINT('Ctrl Pts',(-0.967387853228041,-1.,-1.63013849959083));
#29744=CARTESIAN_POINT('Ctrl Pts',(-0.967387853228041,1.,-1.63013849959083));
#29745=CARTESIAN_POINT('Ctrl Pts',(-0.970669715996356,-1.,-1.63420665729609));
#29746=CARTESIAN_POINT('Ctrl Pts',(-0.970669715996356,1.,-1.63420665729609));
#29747=CARTESIAN_POINT('Ctrl Pts',(-0.974066058287501,-1.,-1.63820952658157));
#29748=CARTESIAN_POINT('Ctrl Pts',(-0.974066058287501,1.,-1.63820952658157));
#29749=CARTESIAN_POINT('Ctrl Pts',(-0.977689794120297,-1.,-1.64233990826831));
#29750=CARTESIAN_POINT('Ctrl Pts',(-0.977689794120297,1.,-1.64233990826831));
#29751=CARTESIAN_POINT('Ctrl Pts',(-0.981562530940574,-1.,-1.64665139190834));
#29752=CARTESIAN_POINT('Ctrl Pts',(-0.981562530940574,1.,-1.64665139190834));
#29753=CARTESIAN_POINT('Ctrl Pts',(-0.985642622921626,-1.,-1.6511001661277));
#29754=CARTESIAN_POINT('Ctrl Pts',(-0.985642622921626,1.,-1.6511001661277));
#29755=CARTESIAN_POINT('Ctrl Pts',(-0.98985562785445,-1.,-1.65559044289746));
#29756=CARTESIAN_POINT('Ctrl Pts',(-0.98985562785445,1.,-1.65559044289746));
#29757=CARTESIAN_POINT('Ctrl Pts',(-0.994121836661116,-1.,-1.66001553809916));
#29758=CARTESIAN_POINT('Ctrl Pts',(-0.994121836661116,1.,-1.66001553809916));
#29759=CARTESIAN_POINT('Ctrl Pts',(-0.998389654952317,-1.,-1.66430758030304));
#29760=CARTESIAN_POINT('Ctrl Pts',(-0.998389654952317,1.,-1.66430758030304));
#29761=CARTESIAN_POINT('Ctrl Pts',(-1.00265091003682,-1.,-1.66846059277231));
#29762=CARTESIAN_POINT('Ctrl Pts',(-1.00265091003682,1.,-1.66846059277231));
#29763=CARTESIAN_POINT('Ctrl Pts',(-1.00692206696387,-1.,-1.67250335383248));
#29764=CARTESIAN_POINT('Ctrl Pts',(-1.00692206696387,1.,-1.67250335383248));
#29765=CARTESIAN_POINT('Ctrl Pts',(-1.01123236493507,-1.,-1.67648246776457));
#29766=CARTESIAN_POINT('Ctrl Pts',(-1.01123236493507,1.,-1.67648246776457));
#29767=CARTESIAN_POINT('Ctrl Pts',(-1.01561026162787,-1.,-1.6804428989482));
#29768=CARTESIAN_POINT('Ctrl Pts',(-1.01561026162787,1.,-1.6804428989482));
#29769=CARTESIAN_POINT('Ctrl Pts',(-1.02006795074222,-1.,-1.68440578021739));
#29770=CARTESIAN_POINT('Ctrl Pts',(-1.02006795074222,1.,-1.68440578021739));
#29771=CARTESIAN_POINT('Ctrl Pts',(-1.02460180535272,-1.,-1.68836910178475));
#29772=CARTESIAN_POINT('Ctrl Pts',(-1.02460180535272,1.,-1.68836910178475));
#29773=CARTESIAN_POINT('Ctrl Pts',(-1.02919977579155,-1.,-1.69231840863471));
#29774=CARTESIAN_POINT('Ctrl Pts',(-1.02919977579155,1.,-1.69231840863471));
#29775=CARTESIAN_POINT('Ctrl Pts',(-1.03384646003587,-1.,-1.69623414782769));
#29776=CARTESIAN_POINT('Ctrl Pts',(-1.03384646003587,1.,-1.69623414782769));
#29777=CARTESIAN_POINT('Ctrl Pts',(-1.03852922490782,-1.,-1.70010052930951));
#29778=CARTESIAN_POINT('Ctrl Pts',(-1.03852922490782,1.,-1.70010052930951));
#29779=CARTESIAN_POINT('Ctrl Pts',(-1.04324363334546,-1.,-1.70391338707969));
#29780=CARTESIAN_POINT('Ctrl Pts',(-1.04324363334546,1.,-1.70391338707969));
#29781=CARTESIAN_POINT('Ctrl Pts',(-1.0479908540499,-1.,-1.70767646263641));
#29782=CARTESIAN_POINT('Ctrl Pts',(-1.0479908540499,1.,-1.70767646263641));
#29783=CARTESIAN_POINT('Ctrl Pts',(-1.05277517202854,-1.,-1.71139783543986));
#29784=CARTESIAN_POINT('Ctrl Pts',(-1.05277517202854,1.,-1.71139783543986));
#29785=CARTESIAN_POINT('Ctrl Pts',(-1.05760163192481,-1.,-1.71508654427022));
#29786=CARTESIAN_POINT('Ctrl Pts',(-1.05760163192481,1.,-1.71508654427022));
#29787=CARTESIAN_POINT('Ctrl Pts',(-1.0624732468065,-1.,-1.71874858456908));
#29788=CARTESIAN_POINT('Ctrl Pts',(-1.0624732468065,1.,-1.71874858456908));
#29789=CARTESIAN_POINT('Ctrl Pts',(-1.06738966975463,-1.,-1.72238500928456));
#29790=CARTESIAN_POINT('Ctrl Pts',(-1.06738966975463,1.,-1.72238500928456));
#29791=CARTESIAN_POINT('Ctrl Pts',(-1.07234866990252,-1.,-1.72599406198489));
#29792=CARTESIAN_POINT('Ctrl Pts',(-1.07234866990252,1.,-1.72599406198489));
#29793=CARTESIAN_POINT('Ctrl Pts',(-1.0773470373727,-1.,-1.72957248977424));
#29794=CARTESIAN_POINT('Ctrl Pts',(-1.0773470373727,1.,-1.72957248977424));
#29795=CARTESIAN_POINT('Ctrl Pts',(-1.08238162784749,-1.,-1.73311705663407));
#29796=CARTESIAN_POINT('Ctrl Pts',(-1.08238162784749,1.,-1.73311705663407));
#29797=CARTESIAN_POINT('Ctrl Pts',(-1.08745056285429,-1.,-1.73662628326093));
#29798=CARTESIAN_POINT('Ctrl Pts',(-1.08745056285429,1.,-1.73662628326093));
#29799=CARTESIAN_POINT('Ctrl Pts',(-1.09255329056496,-1.,-1.74010053962252));
#29800=CARTESIAN_POINT('Ctrl Pts',(-1.09255329056496,1.,-1.74010053962252));
#29801=CARTESIAN_POINT('Ctrl Pts',(-1.09768999241229,-1.,-1.74354119236212));
#29802=CARTESIAN_POINT('Ctrl Pts',(-1.09768999241229,1.,-1.74354119236212));
#29803=CARTESIAN_POINT('Ctrl Pts',(-1.10286118991144,-1.,-1.74695004214924));
#29804=CARTESIAN_POINT('Ctrl Pts',(-1.10286118991144,1.,-1.74695004214924));
#29805=CARTESIAN_POINT('Ctrl Pts',(-1.10806728183003,-1.,-1.75032866075914));
#29806=CARTESIAN_POINT('Ctrl Pts',(-1.10806728183003,1.,-1.75032866075914));
#29807=CARTESIAN_POINT('Ctrl Pts',(-1.11330807582542,-1.,-1.75367772094617));
#29808=CARTESIAN_POINT('Ctrl Pts',(-1.11330807582542,1.,-1.75367772094617));
#29809=CARTESIAN_POINT('Ctrl Pts',(-1.11858293216752,-1.,-1.75699720772089));
#29810=CARTESIAN_POINT('Ctrl Pts',(-1.11858293216752,1.,-1.75699720772089));
#29811=CARTESIAN_POINT('Ctrl Pts',(-1.12389096855078,-1.,-1.76028671825084));
#29812=CARTESIAN_POINT('Ctrl Pts',(-1.12389096855078,1.,-1.76028671825084));
#29813=CARTESIAN_POINT('Ctrl Pts',(-1.12923123555076,-1.,-1.76354571966171));
#29814=CARTESIAN_POINT('Ctrl Pts',(-1.12923123555076,1.,-1.76354571966171));
#29815=CARTESIAN_POINT('Ctrl Pts',(-1.13460291804635,-1.,-1.76677384551883));
#29816=CARTESIAN_POINT('Ctrl Pts',(-1.13460291804635,1.,-1.76677384551883));
#29817=CARTESIAN_POINT('Ctrl Pts',(-1.14000548337,-1.,-1.76997111386806));
#29818=CARTESIAN_POINT('Ctrl Pts',(-1.14000548337,1.,-1.76997111386806));
#29819=CARTESIAN_POINT('Ctrl Pts',(-1.14543858226948,-1.,-1.77313777896234));
#29820=CARTESIAN_POINT('Ctrl Pts',(-1.14543858226948,1.,-1.77313777896234));
#29821=CARTESIAN_POINT('Ctrl Pts',(-1.15090197841531,-1.,-1.77627422557034));
#29822=CARTESIAN_POINT('Ctrl Pts',(-1.15090197841531,1.,-1.77627422557034));
#29823=CARTESIAN_POINT('Ctrl Pts',(-1.15639547194689,-1.,-1.77938085564261));
#29824=CARTESIAN_POINT('Ctrl Pts',(-1.15639547194689,1.,-1.77938085564261));
#29825=CARTESIAN_POINT('Ctrl Pts',(-1.16191881298458,-1.,-1.78245795880949));
#29826=CARTESIAN_POINT('Ctrl Pts',(-1.16191881298458,1.,-1.78245795880949));
#29827=CARTESIAN_POINT('Ctrl Pts',(-1.16747166312239,-1.,-1.78550566040349));
#29828=CARTESIAN_POINT('Ctrl Pts',(-1.16747166312239,1.,-1.78550566040349));
#29829=CARTESIAN_POINT('Ctrl Pts',(-1.17305363177265,-1.,-1.78852398877523));
#29830=CARTESIAN_POINT('Ctrl Pts',(-1.17305363177265,1.,-1.78852398877523));
#29831=CARTESIAN_POINT('Ctrl Pts',(-1.17866429440781,-1.,-1.79151291552646));
#29832=CARTESIAN_POINT('Ctrl Pts',(-1.17866429440781,1.,-1.79151291552646));
#29833=CARTESIAN_POINT('Ctrl Pts',(-1.18430321697471,-1.,-1.79447240321572));
#29834=CARTESIAN_POINT('Ctrl Pts',(-1.18430321697471,1.,-1.79447240321572));
#29835=CARTESIAN_POINT('Ctrl Pts',(-1.1899699793456,-1.,-1.79740245923649));
#29836=CARTESIAN_POINT('Ctrl Pts',(-1.1899699793456,1.,-1.79740245923649));
#29837=CARTESIAN_POINT('Ctrl Pts',(-1.19566418930405,-1.,-1.80030314370121));
#29838=CARTESIAN_POINT('Ctrl Pts',(-1.19566418930405,1.,-1.80030314370121));
#29839=CARTESIAN_POINT('Ctrl Pts',(-1.2013854893912,-1.,-1.8031745483882));
#29840=CARTESIAN_POINT('Ctrl Pts',(-1.2013854893912,1.,-1.8031745483882));
#29841=CARTESIAN_POINT('Ctrl Pts',(-1.20713356605519,-1.,-1.80601678480772));
#29842=CARTESIAN_POINT('Ctrl Pts',(-1.20713356605519,1.,-1.80601678480772));
#29843=CARTESIAN_POINT('Ctrl Pts',(-1.2129081570818,-1.,-1.80882996916931));
#29844=CARTESIAN_POINT('Ctrl Pts',(-1.2129081570818,1.,-1.80882996916931));
#29845=CARTESIAN_POINT('Ctrl Pts',(-1.2187090610323,-1.,-1.81161420806172));
#29846=CARTESIAN_POINT('Ctrl Pts',(-1.2187090610323,1.,-1.81161420806172));
#29847=CARTESIAN_POINT('Ctrl Pts',(-1.22453613304507,-1.,-1.81436959209778));
#29848=CARTESIAN_POINT('Ctrl Pts',(-1.22453613304507,1.,-1.81436959209778));
#29849=CARTESIAN_POINT('Ctrl Pts',(-1.22921864890975,-1.,-1.81655087183054));
#29850=CARTESIAN_POINT('Ctrl Pts',(-1.22921864890975,1.,-1.81655087183054));
#29851=CARTESIAN_POINT('Ctrl Pts',(-1.23274224526804,-1.,-1.81817389920914));
#29852=CARTESIAN_POINT('Ctrl Pts',(-1.23274224526804,1.,-1.81817389920914));
#29853=CARTESIAN_POINT('Ctrl Pts',(-1.23509651170384,-1.,-1.81925017193531));
#29854=CARTESIAN_POINT('Ctrl Pts',(-1.23509651170384,1.,-1.81925017193531));
#29855=CARTESIAN_POINT('Ctrl Pts',(-1.23627494547115,-1.,-1.81978687191668));
#29856=CARTESIAN_POINT('Ctrl Pts',(-1.23627494547115,1.,-1.81978687191668));
#29857=CARTESIAN_POINT('',(-0.892032620296855,1.,-1.5055822144029));
#29858=CARTESIAN_POINT('Ctrl Pts',(-0.892032620296855,1.,-1.5055822144029));
#29859=CARTESIAN_POINT('Ctrl Pts',(-0.894452006967538,1.,-1.50980486807181));
#29860=CARTESIAN_POINT('Ctrl Pts',(-0.89918504749193,1.,-1.51805569591479));
#29861=CARTESIAN_POINT('Ctrl Pts',(-0.905967409640499,1.,-1.52984849890434));
#29862=CARTESIAN_POINT('Ctrl Pts',(-0.91437591904658,1.,-1.54440491152808));
#29863=CARTESIAN_POINT('Ctrl Pts',(-0.923832188966322,1.,-1.56065988582509));
#29864=CARTESIAN_POINT('Ctrl Pts',(-0.932246680128849,1.,-1.57499388385561));
#29865=CARTESIAN_POINT('Ctrl Pts',(-0.939646377909319,1.,-1.58744937489796));
#29866=CARTESIAN_POINT('Ctrl Pts',(-0.946078063325796,1.,-1.59810042045408));
#29867=CARTESIAN_POINT('Ctrl Pts',(-0.951613284361248,1.,-1.60706069897794));
#29868=CARTESIAN_POINT('Ctrl Pts',(-0.956354422921573,1.,-1.61449324337233));
#29869=CARTESIAN_POINT('Ctrl Pts',(-0.960438326099958,1.,-1.62061638139929));
#29870=CARTESIAN_POINT('Ctrl Pts',(-0.964046107037821,1.,-1.6257193066974));
#29871=CARTESIAN_POINT('Ctrl Pts',(-0.967387853228041,1.,-1.63013849959083));
#29872=CARTESIAN_POINT('Ctrl Pts',(-0.970669715996356,1.,-1.63420665729609));
#29873=CARTESIAN_POINT('Ctrl Pts',(-0.974066058287501,1.,-1.63820952658157));
#29874=CARTESIAN_POINT('Ctrl Pts',(-0.977689794120297,1.,-1.64233990826831));
#29875=CARTESIAN_POINT('Ctrl Pts',(-0.981562530940574,1.,-1.64665139190834));
#29876=CARTESIAN_POINT('Ctrl Pts',(-0.985642622921626,1.,-1.6511001661277));
#29877=CARTESIAN_POINT('Ctrl Pts',(-0.98985562785445,1.,-1.65559044289746));
#29878=CARTESIAN_POINT('Ctrl Pts',(-0.994121836661116,1.,-1.66001553809916));
#29879=CARTESIAN_POINT('Ctrl Pts',(-0.998389654952317,1.,-1.66430758030304));
#29880=CARTESIAN_POINT('Ctrl Pts',(-1.00265091003682,1.,-1.66846059277231));
#29881=CARTESIAN_POINT('Ctrl Pts',(-1.00692206696387,1.,-1.67250335383248));
#29882=CARTESIAN_POINT('Ctrl Pts',(-1.01123236493507,1.,-1.67648246776457));
#29883=CARTESIAN_POINT('Ctrl Pts',(-1.01561026162787,1.,-1.6804428989482));
#29884=CARTESIAN_POINT('Ctrl Pts',(-1.02006795074222,1.,-1.68440578021739));
#29885=CARTESIAN_POINT('Ctrl Pts',(-1.02460180535272,1.,-1.68836910178475));
#29886=CARTESIAN_POINT('Ctrl Pts',(-1.02919977579155,1.,-1.69231840863471));
#29887=CARTESIAN_POINT('Ctrl Pts',(-1.03384646003587,1.,-1.69623414782769));
#29888=CARTESIAN_POINT('Ctrl Pts',(-1.03852922490782,1.,-1.70010052930951));
#29889=CARTESIAN_POINT('Ctrl Pts',(-1.04324363334546,1.,-1.70391338707969));
#29890=CARTESIAN_POINT('Ctrl Pts',(-1.0479908540499,1.,-1.70767646263641));
#29891=CARTESIAN_POINT('Ctrl Pts',(-1.05277517202854,1.,-1.71139783543986));
#29892=CARTESIAN_POINT('Ctrl Pts',(-1.05760163192481,1.,-1.71508654427022));
#29893=CARTESIAN_POINT('Ctrl Pts',(-1.0624732468065,1.,-1.71874858456908));
#29894=CARTESIAN_POINT('Ctrl Pts',(-1.06738966975463,1.,-1.72238500928456));
#29895=CARTESIAN_POINT('Ctrl Pts',(-1.07234866990252,1.,-1.72599406198489));
#29896=CARTESIAN_POINT('Ctrl Pts',(-1.0773470373727,1.,-1.72957248977424));
#29897=CARTESIAN_POINT('Ctrl Pts',(-1.08238162784749,1.,-1.73311705663407));
#29898=CARTESIAN_POINT('Ctrl Pts',(-1.08745056285429,1.,-1.73662628326093));
#29899=CARTESIAN_POINT('Ctrl Pts',(-1.09255329056496,1.,-1.74010053962252));
#29900=CARTESIAN_POINT('Ctrl Pts',(-1.09768999241229,1.,-1.74354119236212));
#29901=CARTESIAN_POINT('Ctrl Pts',(-1.10286118991144,1.,-1.74695004214924));
#29902=CARTESIAN_POINT('Ctrl Pts',(-1.10806728183003,1.,-1.75032866075914));
#29903=CARTESIAN_POINT('Ctrl Pts',(-1.11330807582542,1.,-1.75367772094617));
#29904=CARTESIAN_POINT('Ctrl Pts',(-1.11858293216752,1.,-1.75699720772089));
#29905=CARTESIAN_POINT('Ctrl Pts',(-1.12389096855078,1.,-1.76028671825084));
#29906=CARTESIAN_POINT('Ctrl Pts',(-1.12923123555076,1.,-1.76354571966171));
#29907=CARTESIAN_POINT('Ctrl Pts',(-1.13460291804635,1.,-1.76677384551883));
#29908=CARTESIAN_POINT('Ctrl Pts',(-1.14000548337,1.,-1.76997111386806));
#29909=CARTESIAN_POINT('Ctrl Pts',(-1.14543858226948,1.,-1.77313777896234));
#29910=CARTESIAN_POINT('Ctrl Pts',(-1.15090197841531,1.,-1.77627422557034));
#29911=CARTESIAN_POINT('Ctrl Pts',(-1.15639547194689,1.,-1.77938085564261));
#29912=CARTESIAN_POINT('Ctrl Pts',(-1.16191881298458,1.,-1.78245795880949));
#29913=CARTESIAN_POINT('Ctrl Pts',(-1.16747166312239,1.,-1.78550566040349));
#29914=CARTESIAN_POINT('Ctrl Pts',(-1.17305363177265,1.,-1.78852398877523));
#29915=CARTESIAN_POINT('Ctrl Pts',(-1.17866429440781,1.,-1.79151291552646));
#29916=CARTESIAN_POINT('Ctrl Pts',(-1.18430321697471,1.,-1.79447240321572));
#29917=CARTESIAN_POINT('Ctrl Pts',(-1.1899699793456,1.,-1.79740245923649));
#29918=CARTESIAN_POINT('Ctrl Pts',(-1.19566418930405,1.,-1.80030314370121));
#29919=CARTESIAN_POINT('Ctrl Pts',(-1.2013854893912,1.,-1.8031745483882));
#29920=CARTESIAN_POINT('Ctrl Pts',(-1.20713356605519,1.,-1.80601678480772));
#29921=CARTESIAN_POINT('Ctrl Pts',(-1.2129081570818,1.,-1.80882996916931));
#29922=CARTESIAN_POINT('Ctrl Pts',(-1.2187090610323,1.,-1.81161420806172));
#29923=CARTESIAN_POINT('Ctrl Pts',(-1.22453613304507,1.,-1.81436959209778));
#29924=CARTESIAN_POINT('Ctrl Pts',(-1.22921864890975,1.,-1.81655087183054));
#29925=CARTESIAN_POINT('Ctrl Pts',(-1.23274224526804,1.,-1.81817389920914));
#29926=CARTESIAN_POINT('Ctrl Pts',(-1.23509651170384,1.,-1.81925017193531));
#29927=CARTESIAN_POINT('Ctrl Pts',(-1.23627494547115,1.,-1.81978687191668));
#29928=CARTESIAN_POINT('',(-0.892032620296856,0.,-1.5055822144029));
#29929=CARTESIAN_POINT('Origin',(0.,0.,0.));
#29930=CARTESIAN_POINT('',(-0.693717979106305,1.,-1.60662857109684));
#29931=CARTESIAN_POINT('Origin',(0.,1.,0.));
#29932=CARTESIAN_POINT('',(-0.693717979106306,0.,-1.60662857109684));
#29933=CARTESIAN_POINT('Ctrl Pts',(-0.745574324794401,-1.,-2.0698113262342));
#29934=CARTESIAN_POINT('Ctrl Pts',(-0.745574324794401,1.,-2.0698113262342));
#29935=CARTESIAN_POINT('Ctrl Pts',(-0.745832791378367,-1.,-2.06854248895728));
#29936=CARTESIAN_POINT('Ctrl Pts',(-0.745832791378367,1.,-2.06854248895728));
#29937=CARTESIAN_POINT('Ctrl Pts',(-0.7463458715442,-1.,-2.06600523016815));
#29938=CARTESIAN_POINT('Ctrl Pts',(-0.7463458715442,1.,-2.06600523016815));
#29939=CARTESIAN_POINT('Ctrl Pts',(-0.747103932787919,-1.,-2.06220058927826));
#29940=CARTESIAN_POINT('Ctrl Pts',(-0.747103932787919,1.,-2.06220058927826));
#29941=CARTESIAN_POINT('Ctrl Pts',(-0.748091554183802,-1.,-2.05713023031006));
#29942=CARTESIAN_POINT('Ctrl Pts',(-0.748091554183802,1.,-2.05713023031006));
#29943=CARTESIAN_POINT('Ctrl Pts',(-0.749287468665046,-1.,-2.05079645592154));
#29944=CARTESIAN_POINT('Ctrl Pts',(-0.749287468665046,1.,-2.05079645592154));
#29945=CARTESIAN_POINT('Ctrl Pts',(-0.750444657875576,-1.,-2.04446689147979));
#29946=CARTESIAN_POINT('Ctrl Pts',(-0.750444657875576,1.,-2.04446689147979));
#29947=CARTESIAN_POINT('Ctrl Pts',(-0.751562963361115,-1.,-2.03814160092099));
#29948=CARTESIAN_POINT('Ctrl Pts',(-0.751562963361115,1.,-2.03814160092099));
#29949=CARTESIAN_POINT('Ctrl Pts',(-0.752642180487211,-1.,-2.03182068456221));
#29950=CARTESIAN_POINT('Ctrl Pts',(-0.752642180487211,1.,-2.03182068456221));
#29951=CARTESIAN_POINT('Ctrl Pts',(-0.753682061112768,-1.,-2.02550428623313));
#29952=CARTESIAN_POINT('Ctrl Pts',(-0.753682061112768,1.,-2.02550428623313));
#29953=CARTESIAN_POINT('Ctrl Pts',(-0.754682330722816,-1.,-2.01919259405809));
#29954=CARTESIAN_POINT('Ctrl Pts',(-0.754682330722816,1.,-2.01919259405809));
#29955=CARTESIAN_POINT('Ctrl Pts',(-0.755642704957865,-1.,-2.01288584328084));
#29956=CARTESIAN_POINT('Ctrl Pts',(-0.755642704957865,1.,-2.01288584328084));
#29957=CARTESIAN_POINT('Ctrl Pts',(-0.75656290464667,-1.,-2.0065843158773));
#29958=CARTESIAN_POINT('Ctrl Pts',(-0.75656290464667,1.,-2.0065843158773));
#29959=CARTESIAN_POINT('Ctrl Pts',(-0.757442676862724,-1.,-2.00028834739178));
#29960=CARTESIAN_POINT('Ctrl Pts',(-0.757442676862724,1.,-2.00028834739178));
#29961=CARTESIAN_POINT('Ctrl Pts',(-0.758281796766761,-1.,-1.99399831098817));
#29962=CARTESIAN_POINT('Ctrl Pts',(-0.758281796766761,1.,-1.99399831098817));
#29963=CARTESIAN_POINT('Ctrl Pts',(-0.759080037802488,-1.,-1.98771456680874));
#29964=CARTESIAN_POINT('Ctrl Pts',(-0.759080037802488,1.,-1.98771456680874));
#29965=CARTESIAN_POINT('Ctrl Pts',(-0.75983714745219,-1.,-1.98143741418172));
#29966=CARTESIAN_POINT('Ctrl Pts',(-0.75983714745219,1.,-1.98143741418172));
#29967=CARTESIAN_POINT('Ctrl Pts',(-0.760552825409757,-1.,-1.97516705321494));
#29968=CARTESIAN_POINT('Ctrl Pts',(-0.760552825409757,1.,-1.97516705321494));
#29969=CARTESIAN_POINT('Ctrl Pts',(-0.76122669048382,-1.,-1.96890351582499));
#29970=CARTESIAN_POINT('Ctrl Pts',(-0.76122669048382,1.,-1.96890351582499));
#29971=CARTESIAN_POINT('Ctrl Pts',(-0.761858300014423,-1.,-1.96264672744186));
#29972=CARTESIAN_POINT('Ctrl Pts',(-0.761858300014423,1.,-1.96264672744186));
#29973=CARTESIAN_POINT('Ctrl Pts',(-0.762447203806179,-1.,-1.95639665309869));
#29974=CARTESIAN_POINT('Ctrl Pts',(-0.762447203806179,1.,-1.95639665309869));
#29975=CARTESIAN_POINT('Ctrl Pts',(-0.762992990878769,-1.,-1.95015342590024));
#29976=CARTESIAN_POINT('Ctrl Pts',(-0.762992990878769,1.,-1.95015342590024));
#29977=CARTESIAN_POINT('Ctrl Pts',(-0.763495333538629,-1.,-1.9439174661764));
#29978=CARTESIAN_POINT('Ctrl Pts',(-0.763495333538629,1.,-1.9439174661764));
#29979=CARTESIAN_POINT('Ctrl Pts',(-0.763954049121458,-1.,-1.93768964875886));
#29980=CARTESIAN_POINT('Ctrl Pts',(-0.763954049121458,1.,-1.93768964875886));
#29981=CARTESIAN_POINT('Ctrl Pts',(-0.764369010673941,-1.,-1.93147105496382));
#29982=CARTESIAN_POINT('Ctrl Pts',(-0.764369010673941,1.,-1.93147105496382));
#29983=CARTESIAN_POINT('Ctrl Pts',(-0.764740025488211,-1.,-1.92526263537048));
#29984=CARTESIAN_POINT('Ctrl Pts',(-0.764740025488211,1.,-1.92526263537048));
#29985=CARTESIAN_POINT('Ctrl Pts',(-0.765066729667088,-1.,-1.91906491634196));
#29986=CARTESIAN_POINT('Ctrl Pts',(-0.765066729667088,1.,-1.91906491634196));
#29987=CARTESIAN_POINT('Ctrl Pts',(-0.765348465884722,-1.,-1.91287765805169));
#29988=CARTESIAN_POINT('Ctrl Pts',(-0.765348465884722,1.,-1.91287765805169));
#29989=CARTESIAN_POINT('Ctrl Pts',(-0.765584196937919,-1.,-1.90669961402356));
#29990=CARTESIAN_POINT('Ctrl Pts',(-0.765584196937919,1.,-1.90669961402356));
#29991=CARTESIAN_POINT('Ctrl Pts',(-0.765772772593386,-1.,-1.90052930393596));
#29992=CARTESIAN_POINT('Ctrl Pts',(-0.765772772593386,1.,-1.90052930393596));
#29993=CARTESIAN_POINT('Ctrl Pts',(-0.765913193856978,-1.,-1.89436577771388));
#29994=CARTESIAN_POINT('Ctrl Pts',(-0.765913193856978,1.,-1.89436577771388));
#29995=CARTESIAN_POINT('Ctrl Pts',(-0.766004837062091,-1.,-1.88820926433409));
#29996=CARTESIAN_POINT('Ctrl Pts',(-0.766004837062091,1.,-1.88820926433409));
#29997=CARTESIAN_POINT('Ctrl Pts',(-0.766047794851865,-1.,-1.88206215302561));
#29998=CARTESIAN_POINT('Ctrl Pts',(-0.766047794851865,1.,-1.88206215302561));
#29999=CARTESIAN_POINT('Ctrl Pts',(-0.766042837036744,-1.,-1.87592888967883));
#30000=CARTESIAN_POINT('Ctrl Pts',(-0.766042837036744,1.,-1.87592888967883));
#30001=CARTESIAN_POINT('Ctrl Pts',(-0.765990708546091,-1.,-1.86981398314341));
#30002=CARTESIAN_POINT('Ctrl Pts',(-0.765990708546091,1.,-1.86981398314341));
#30003=CARTESIAN_POINT('Ctrl Pts',(-0.765891519092547,-1.,-1.86372027063312));
#30004=CARTESIAN_POINT('Ctrl Pts',(-0.765891519092547,1.,-1.86372027063312));
#30005=CARTESIAN_POINT('Ctrl Pts',(-0.765744212909318,-1.,-1.85764741390394));
#30006=CARTESIAN_POINT('Ctrl Pts',(-0.765744212909318,1.,-1.85764741390394));
#30007=CARTESIAN_POINT('Ctrl Pts',(-0.765545710619062,-1.,-1.85158945130063));
#30008=CARTESIAN_POINT('Ctrl Pts',(-0.765545710619062,1.,-1.85158945130063));
#30009=CARTESIAN_POINT('Ctrl Pts',(-0.765291664862029,-1.,-1.84553698875924));
#30010=CARTESIAN_POINT('Ctrl Pts',(-0.765291664862029,1.,-1.84553698875924));
#30011=CARTESIAN_POINT('Ctrl Pts',(-0.764978057881737,-1.,-1.83948181064835));
#30012=CARTESIAN_POINT('Ctrl Pts',(-0.764978057881737,1.,-1.83948181064835));
#30013=CARTESIAN_POINT('Ctrl Pts',(-0.764602549687853,-1.,-1.83342077227142));
#30014=CARTESIAN_POINT('Ctrl Pts',(-0.764602549687853,1.,-1.83342077227142));
#30015=CARTESIAN_POINT('Ctrl Pts',(-0.764165902605995,-1.,-1.82735991200065));
#30016=CARTESIAN_POINT('Ctrl Pts',(-0.764165902605995,1.,-1.82735991200065));
#30017=CARTESIAN_POINT('Ctrl Pts',(-0.763673465462726,-1.,-1.82131873145266));
#30018=CARTESIAN_POINT('Ctrl Pts',(-0.763673465462726,1.,-1.82131873145266));
#30019=CARTESIAN_POINT('Ctrl Pts',(-0.763132003836634,-1.,-1.8153211840553));
#30020=CARTESIAN_POINT('Ctrl Pts',(-0.763132003836634,1.,-1.8153211840553));
#30021=CARTESIAN_POINT('Ctrl Pts',(-0.762546129463938,-1.,-1.80938551463965));
#30022=CARTESIAN_POINT('Ctrl Pts',(-0.762546129463938,1.,-1.80938551463965));
#30023=CARTESIAN_POINT('Ctrl Pts',(-0.761915336443547,-1.,-1.80351583877342));
#30024=CARTESIAN_POINT('Ctrl Pts',(-0.761915336443547,1.,-1.80351583877342));
#30025=CARTESIAN_POINT('Ctrl Pts',(-0.761229695230558,-1.,-1.79768986997783));
#30026=CARTESIAN_POINT('Ctrl Pts',(-0.761229695230558,1.,-1.79768986997783));
#30027=CARTESIAN_POINT('Ctrl Pts',(-0.760469555880749,-1.,-1.7918581561088));
#30028=CARTESIAN_POINT('Ctrl Pts',(-0.760469555880749,1.,-1.7918581561088));
#30029=CARTESIAN_POINT('Ctrl Pts',(-0.759614401110189,-1.,-1.78596964884604));
#30030=CARTESIAN_POINT('Ctrl Pts',(-0.759614401110189,1.,-1.78596964884604));
#30031=CARTESIAN_POINT('Ctrl Pts',(-0.758650626677518,-1.,-1.77999411220945));
#30032=CARTESIAN_POINT('Ctrl Pts',(-0.758650626677518,1.,-1.77999411220945));
#30033=CARTESIAN_POINT('Ctrl Pts',(-0.757578264077029,-1.,-1.77394167108292));
#30034=CARTESIAN_POINT('Ctrl Pts',(-0.757578264077029,1.,-1.77394167108292));
#30035=CARTESIAN_POINT('Ctrl Pts',(-0.75642189602781,-1.,-1.76789396002998));
#30036=CARTESIAN_POINT('Ctrl Pts',(-0.75642189602781,1.,-1.76789396002998));
#30037=CARTESIAN_POINT('Ctrl Pts',(-0.755220979974461,-1.,-1.76197817240128));
#30038=CARTESIAN_POINT('Ctrl Pts',(-0.755220979974461,1.,-1.76197817240128));
#30039=CARTESIAN_POINT('Ctrl Pts',(-0.754009254027829,-1.,-1.75631083600019));
#30040=CARTESIAN_POINT('Ctrl Pts',(-0.754009254027829,1.,-1.75631083600019));
#30041=CARTESIAN_POINT('Ctrl Pts',(-0.752797683531314,-1.,-1.75095139468794));
#30042=CARTESIAN_POINT('Ctrl Pts',(-0.752797683531314,1.,-1.75095139468794));
#30043=CARTESIAN_POINT('Ctrl Pts',(-0.751555614164482,-1.,-1.74585086852502));
#30044=CARTESIAN_POINT('Ctrl Pts',(-0.751555614164482,1.,-1.74585086852502));
#30045=CARTESIAN_POINT('Ctrl Pts',(-0.750193435981249,-1.,-1.74080458267114));
#30046=CARTESIAN_POINT('Ctrl Pts',(-0.750193435981249,1.,-1.74080458267114));
#30047=CARTESIAN_POINT('Ctrl Pts',(-0.74858246295687,-1.,-1.7355035168033));
#30048=CARTESIAN_POINT('Ctrl Pts',(-0.74858246295687,1.,-1.7355035168033));
#30049=CARTESIAN_POINT('Ctrl Pts',(-0.746574710097752,-1.,-1.72958533647714));
#30050=CARTESIAN_POINT('Ctrl Pts',(-0.746574710097752,1.,-1.72958533647714));
#30051=CARTESIAN_POINT('Ctrl Pts',(-0.744021445433093,-1.,-1.72268229916769));
#30052=CARTESIAN_POINT('Ctrl Pts',(-0.744021445433093,1.,-1.72268229916769));
#30053=CARTESIAN_POINT('Ctrl Pts',(-0.74079516202821,-1.,-1.71447789751001));
#30054=CARTESIAN_POINT('Ctrl Pts',(-0.74079516202821,1.,-1.71447789751001));
#30055=CARTESIAN_POINT('Ctrl Pts',(-0.736799665716932,-1.,-1.70473309004249));
#30056=CARTESIAN_POINT('Ctrl Pts',(-0.736799665716932,1.,-1.70473309004249));
#30057=CARTESIAN_POINT('Ctrl Pts',(-0.731963238685357,-1.,-1.69326921972915));
#30058=CARTESIAN_POINT('Ctrl Pts',(-0.731963238685357,1.,-1.69326921972915));
#30059=CARTESIAN_POINT('Ctrl Pts',(-0.726235967982445,-1.,-1.67996158451922));
#30060=CARTESIAN_POINT('Ctrl Pts',(-0.726235967982445,1.,-1.67996158451922));
#30061=CARTESIAN_POINT('Ctrl Pts',(-0.71958543378795,-1.,-1.66472880551777));
#30062=CARTESIAN_POINT('Ctrl Pts',(-0.71958543378795,1.,-1.66472880551777));
#30063=CARTESIAN_POINT('Ctrl Pts',(-0.711993139340447,-1.,-1.64752408828442));
#30064=CARTESIAN_POINT('Ctrl Pts',(-0.711993139340447,1.,-1.64752408828442));
#30065=CARTESIAN_POINT('Ctrl Pts',(-0.705159151977294,-1.,-1.6321654166204));
#30066=CARTESIAN_POINT('Ctrl Pts',(-0.705159151977294,1.,-1.6321654166204));
#30067=CARTESIAN_POINT('Ctrl Pts',(-0.699605146398837,-1.,-1.61974673471117));
#30068=CARTESIAN_POINT('Ctrl Pts',(-0.699605146398837,1.,-1.61974673471117));
#30069=CARTESIAN_POINT('Ctrl Pts',(-0.69571209787897,-1.,-1.61106790957619));
#30070=CARTESIAN_POINT('Ctrl Pts',(-0.69571209787897,1.,-1.61106790957619));
#30071=CARTESIAN_POINT('Ctrl Pts',(-0.693717979106305,-1.,-1.60662857109684));
#30072=CARTESIAN_POINT('Ctrl Pts',(-0.693717979106305,1.,-1.60662857109684));
#30073=CARTESIAN_POINT('',(-0.745574324794401,1.,-2.0698113262342));
#30074=CARTESIAN_POINT('Ctrl Pts',(-0.745574324794401,1.,-2.0698113262342));
#30075=CARTESIAN_POINT('Ctrl Pts',(-0.745832791378367,1.,-2.06854248895728));
#30076=CARTESIAN_POINT('Ctrl Pts',(-0.7463458715442,1.,-2.06600523016815));
#30077=CARTESIAN_POINT('Ctrl Pts',(-0.747103932787919,1.,-2.06220058927826));
#30078=CARTESIAN_POINT('Ctrl Pts',(-0.748091554183802,1.,-2.05713023031006));
#30079=CARTESIAN_POINT('Ctrl Pts',(-0.749287468665046,1.,-2.05079645592154));
#30080=CARTESIAN_POINT('Ctrl Pts',(-0.750444657875576,1.,-2.04446689147979));
#30081=CARTESIAN_POINT('Ctrl Pts',(-0.751562963361115,1.,-2.03814160092099));
#30082=CARTESIAN_POINT('Ctrl Pts',(-0.752642180487211,1.,-2.03182068456221));
#30083=CARTESIAN_POINT('Ctrl Pts',(-0.753682061112768,1.,-2.02550428623313));
#30084=CARTESIAN_POINT('Ctrl Pts',(-0.754682330722816,1.,-2.01919259405809));
#30085=CARTESIAN_POINT('Ctrl Pts',(-0.755642704957865,1.,-2.01288584328084));
#30086=CARTESIAN_POINT('Ctrl Pts',(-0.75656290464667,1.,-2.0065843158773));
#30087=CARTESIAN_POINT('Ctrl Pts',(-0.757442676862724,1.,-2.00028834739178));
#30088=CARTESIAN_POINT('Ctrl Pts',(-0.758281796766761,1.,-1.99399831098817));
#30089=CARTESIAN_POINT('Ctrl Pts',(-0.759080037802488,1.,-1.98771456680874));
#30090=CARTESIAN_POINT('Ctrl Pts',(-0.75983714745219,1.,-1.98143741418172));
#30091=CARTESIAN_POINT('Ctrl Pts',(-0.760552825409757,1.,-1.97516705321494));
#30092=CARTESIAN_POINT('Ctrl Pts',(-0.76122669048382,1.,-1.96890351582499));
#30093=CARTESIAN_POINT('Ctrl Pts',(-0.761858300014423,1.,-1.96264672744186));
#30094=CARTESIAN_POINT('Ctrl Pts',(-0.762447203806179,1.,-1.95639665309869));
#30095=CARTESIAN_POINT('Ctrl Pts',(-0.762992990878769,1.,-1.95015342590024));
#30096=CARTESIAN_POINT('Ctrl Pts',(-0.763495333538629,1.,-1.9439174661764));
#30097=CARTESIAN_POINT('Ctrl Pts',(-0.763954049121458,1.,-1.93768964875886));
#30098=CARTESIAN_POINT('Ctrl Pts',(-0.764369010673941,1.,-1.93147105496382));
#30099=CARTESIAN_POINT('Ctrl Pts',(-0.764740025488211,1.,-1.92526263537048));
#30100=CARTESIAN_POINT('Ctrl Pts',(-0.765066729667088,1.,-1.91906491634196));
#30101=CARTESIAN_POINT('Ctrl Pts',(-0.765348465884722,1.,-1.91287765805169));
#30102=CARTESIAN_POINT('Ctrl Pts',(-0.765584196937919,1.,-1.90669961402356));
#30103=CARTESIAN_POINT('Ctrl Pts',(-0.765772772593386,1.,-1.90052930393596));
#30104=CARTESIAN_POINT('Ctrl Pts',(-0.765913193856978,1.,-1.89436577771388));
#30105=CARTESIAN_POINT('Ctrl Pts',(-0.766004837062091,1.,-1.88820926433409));
#30106=CARTESIAN_POINT('Ctrl Pts',(-0.766047794851865,1.,-1.88206215302561));
#30107=CARTESIAN_POINT('Ctrl Pts',(-0.766042837036744,1.,-1.87592888967883));
#30108=CARTESIAN_POINT('Ctrl Pts',(-0.765990708546091,1.,-1.86981398314341));
#30109=CARTESIAN_POINT('Ctrl Pts',(-0.765891519092547,1.,-1.86372027063312));
#30110=CARTESIAN_POINT('Ctrl Pts',(-0.765744212909318,1.,-1.85764741390394));
#30111=CARTESIAN_POINT('Ctrl Pts',(-0.765545710619062,1.,-1.85158945130063));
#30112=CARTESIAN_POINT('Ctrl Pts',(-0.765291664862029,1.,-1.84553698875924));
#30113=CARTESIAN_POINT('Ctrl Pts',(-0.764978057881737,1.,-1.83948181064835));
#30114=CARTESIAN_POINT('Ctrl Pts',(-0.764602549687853,1.,-1.83342077227142));
#30115=CARTESIAN_POINT('Ctrl Pts',(-0.764165902605995,1.,-1.82735991200065));
#30116=CARTESIAN_POINT('Ctrl Pts',(-0.763673465462726,1.,-1.82131873145266));
#30117=CARTESIAN_POINT('Ctrl Pts',(-0.763132003836634,1.,-1.8153211840553));
#30118=CARTESIAN_POINT('Ctrl Pts',(-0.762546129463938,1.,-1.80938551463965));
#30119=CARTESIAN_POINT('Ctrl Pts',(-0.761915336443547,1.,-1.80351583877342));
#30120=CARTESIAN_POINT('Ctrl Pts',(-0.761229695230558,1.,-1.79768986997783));
#30121=CARTESIAN_POINT('Ctrl Pts',(-0.760469555880749,1.,-1.7918581561088));
#30122=CARTESIAN_POINT('Ctrl Pts',(-0.759614401110189,1.,-1.78596964884604));
#30123=CARTESIAN_POINT('Ctrl Pts',(-0.758650626677518,1.,-1.77999411220945));
#30124=CARTESIAN_POINT('Ctrl Pts',(-0.757578264077029,1.,-1.77394167108292));
#30125=CARTESIAN_POINT('Ctrl Pts',(-0.75642189602781,1.,-1.76789396002998));
#30126=CARTESIAN_POINT('Ctrl Pts',(-0.755220979974461,1.,-1.76197817240128));
#30127=CARTESIAN_POINT('Ctrl Pts',(-0.754009254027829,1.,-1.75631083600019));
#30128=CARTESIAN_POINT('Ctrl Pts',(-0.752797683531314,1.,-1.75095139468794));
#30129=CARTESIAN_POINT('Ctrl Pts',(-0.751555614164482,1.,-1.74585086852502));
#30130=CARTESIAN_POINT('Ctrl Pts',(-0.750193435981249,1.,-1.74080458267114));
#30131=CARTESIAN_POINT('Ctrl Pts',(-0.74858246295687,1.,-1.7355035168033));
#30132=CARTESIAN_POINT('Ctrl Pts',(-0.746574710097752,1.,-1.72958533647714));
#30133=CARTESIAN_POINT('Ctrl Pts',(-0.744021445433093,1.,-1.72268229916769));
#30134=CARTESIAN_POINT('Ctrl Pts',(-0.74079516202821,1.,-1.71447789751001));
#30135=CARTESIAN_POINT('Ctrl Pts',(-0.736799665716932,1.,-1.70473309004249));
#30136=CARTESIAN_POINT('Ctrl Pts',(-0.731963238685357,1.,-1.69326921972915));
#30137=CARTESIAN_POINT('Ctrl Pts',(-0.726235967982445,1.,-1.67996158451922));
#30138=CARTESIAN_POINT('Ctrl Pts',(-0.71958543378795,1.,-1.66472880551777));
#30139=CARTESIAN_POINT('Ctrl Pts',(-0.711993139340447,1.,-1.64752408828442));
#30140=CARTESIAN_POINT('Ctrl Pts',(-0.705159151977294,1.,-1.6321654166204));
#30141=CARTESIAN_POINT('Ctrl Pts',(-0.699605146398837,1.,-1.61974673471117));
#30142=CARTESIAN_POINT('Ctrl Pts',(-0.69571209787897,1.,-1.61106790957619));
#30143=CARTESIAN_POINT('Ctrl Pts',(-0.693717979106305,1.,-1.60662857109684));
#30144=CARTESIAN_POINT('',(-0.745574324794401,0.,-2.0698113262342));
#30145=CARTESIAN_POINT('Origin',(-0.61342227326009,0.,-2.11275013067528));
#30146=CARTESIAN_POINT('',(-0.61342227326009,1.,-2.11275013067528));
#30147=CARTESIAN_POINT('',(-0.745574324794401,1.,-2.0698113262342));
#30148=CARTESIAN_POINT('',(-0.61342227326009,0.,-2.11275013067528));
#30149=CARTESIAN_POINT('Ctrl Pts',(-0.383122945602004,-1.,-1.7075470150345));
#30150=CARTESIAN_POINT('Ctrl Pts',(-0.383122945602004,1.,-1.7075470150345));
#30151=CARTESIAN_POINT('Ctrl Pts',(-0.384119047315542,-1.,-1.71231062891958));
#30152=CARTESIAN_POINT('Ctrl Pts',(-0.384119047315542,1.,-1.71231062891958));
#30153=CARTESIAN_POINT('Ctrl Pts',(-0.38607079032701,-1.,-1.72162022246158));
#30154=CARTESIAN_POINT('Ctrl Pts',(-0.38607079032701,1.,-1.72162022246158));
#30155=CARTESIAN_POINT('Ctrl Pts',(-0.388877023509191,-1.,-1.7349317097561));
#30156=CARTESIAN_POINT('Ctrl Pts',(-0.388877023509191,1.,-1.7349317097561));
#30157=CARTESIAN_POINT('Ctrl Pts',(-0.392375812294307,-1.,-1.75137405313962));
#30158=CARTESIAN_POINT('Ctrl Pts',(-0.392375812294307,1.,-1.75137405313962));
#30159=CARTESIAN_POINT('Ctrl Pts',(-0.39634619612042,-1.,-1.7697556004756));
#30160=CARTESIAN_POINT('Ctrl Pts',(-0.39634619612042,1.,-1.7697556004756));
#30161=CARTESIAN_POINT('Ctrl Pts',(-0.39991940378308,-1.,-1.78598826347533));
#30162=CARTESIAN_POINT('Ctrl Pts',(-0.39991940378308,1.,-1.78598826347533));
#30163=CARTESIAN_POINT('Ctrl Pts',(-0.403107976170441,-1.,-1.80012077176221));
#30164=CARTESIAN_POINT('Ctrl Pts',(-0.403107976170441,1.,-1.80012077176221));
#30165=CARTESIAN_POINT('Ctrl Pts',(-0.405933518411838,-1.,-1.81223801813988));
#30166=CARTESIAN_POINT('Ctrl Pts',(-0.405933518411838,1.,-1.81223801813988));
#30167=CARTESIAN_POINT('Ctrl Pts',(-0.408428948108533,-1.,-1.8224702267854));
#30168=CARTESIAN_POINT('Ctrl Pts',(-0.408428948108533,1.,-1.8224702267854));
#30169=CARTESIAN_POINT('Ctrl Pts',(-0.410641256301675,-1.,-1.83100408895216));
#30170=CARTESIAN_POINT('Ctrl Pts',(-0.410641256301675,1.,-1.83100408895216));
#30171=CARTESIAN_POINT('Ctrl Pts',(-0.412633125322162,-1.,-1.83808953475839));
#30172=CARTESIAN_POINT('Ctrl Pts',(-0.412633125322162,1.,-1.83808953475839));
#30173=CARTESIAN_POINT('Ctrl Pts',(-0.41448743825434,-1.,-1.8440575707371));
#30174=CARTESIAN_POINT('Ctrl Pts',(-0.41448743825434,1.,-1.8440575707371));
#30175=CARTESIAN_POINT('Ctrl Pts',(-0.416300022038864,-1.,-1.84929312929882));
#30176=CARTESIAN_POINT('Ctrl Pts',(-0.416300022038864,1.,-1.84929312929882));
#30177=CARTESIAN_POINT('Ctrl Pts',(-0.418164129143534,-1.,-1.85417632856234));
#30178=CARTESIAN_POINT('Ctrl Pts',(-0.418164129143534,1.,-1.85417632856234));
#30179=CARTESIAN_POINT('Ctrl Pts',(-0.420157287975619,-1.,-1.85903281096686));
#30180=CARTESIAN_POINT('Ctrl Pts',(-0.420157287975619,1.,-1.85903281096686));
#30181=CARTESIAN_POINT('Ctrl Pts',(-0.422327307418275,-1.,-1.86408083334028));
#30182=CARTESIAN_POINT('Ctrl Pts',(-0.422327307418275,1.,-1.86408083334028));
#30183=CARTESIAN_POINT('Ctrl Pts',(-0.424678177291359,-1.,-1.86937803944323));
#30184=CARTESIAN_POINT('Ctrl Pts',(-0.424678177291359,1.,-1.86937803944323));
#30185=CARTESIAN_POINT('Ctrl Pts',(-0.427183828519102,-1.,-1.87486989291484));
#30186=CARTESIAN_POINT('Ctrl Pts',(-0.427183828519102,1.,-1.87486989291484));
#30187=CARTESIAN_POINT('Ctrl Pts',(-0.429803062482344,-1.,-1.88044229001832));
#30188=CARTESIAN_POINT('Ctrl Pts',(-0.429803062482344,1.,-1.88044229001832));
#30189=CARTESIAN_POINT('Ctrl Pts',(-0.432493038548748,-1.,-1.88596913666793));
#30190=CARTESIAN_POINT('Ctrl Pts',(-0.432493038548748,1.,-1.88596913666793));
#30191=CARTESIAN_POINT('Ctrl Pts',(-0.435225660963383,-1.,-1.89136993975504));
#30192=CARTESIAN_POINT('Ctrl Pts',(-0.435225660963383,1.,-1.89136993975504));
#30193=CARTESIAN_POINT('Ctrl Pts',(-0.437995003948244,-1.,-1.89663648956466));
#30194=CARTESIAN_POINT('Ctrl Pts',(-0.437995003948244,1.,-1.89663648956466));
#30195=CARTESIAN_POINT('Ctrl Pts',(-0.440807833704038,-1.,-1.90180124389086));
#30196=CARTESIAN_POINT('Ctrl Pts',(-0.440807833704038,1.,-1.90180124389086));
#30197=CARTESIAN_POINT('Ctrl Pts',(-0.443677556849151,-1.,-1.90691756144898));
#30198=CARTESIAN_POINT('Ctrl Pts',(-0.443677556849151,1.,-1.90691756144898));
#30199=CARTESIAN_POINT('Ctrl Pts',(-0.446617343485711,-1.,-1.9120369998112));
#30200=CARTESIAN_POINT('Ctrl Pts',(-0.446617343485711,1.,-1.9120369998112));
#30201=CARTESIAN_POINT('Ctrl Pts',(-0.449632260106662,-1.,-1.91718342555755));
#30202=CARTESIAN_POINT('Ctrl Pts',(-0.449632260106662,1.,-1.91718342555755));
#30203=CARTESIAN_POINT('Ctrl Pts',(-0.452719478359432,-1.,-1.92235380648502));
#30204=CARTESIAN_POINT('Ctrl Pts',(-0.452719478359432,1.,-1.92235380648502));
#30205=CARTESIAN_POINT('Ctrl Pts',(-0.455872005174371,-1.,-1.92753067150476));
#30206=CARTESIAN_POINT('Ctrl Pts',(-0.455872005174371,1.,-1.92753067150476));
#30207=CARTESIAN_POINT('Ctrl Pts',(-0.459081234547926,-1.,-1.93269066517934));
#30208=CARTESIAN_POINT('Ctrl Pts',(-0.459081234547926,1.,-1.93269066517934));
#30209=CARTESIAN_POINT('Ctrl Pts',(-0.462340031009056,-1.,-1.93781486640821));
#30210=CARTESIAN_POINT('Ctrl Pts',(-0.462340031009056,1.,-1.93781486640821));
#30211=CARTESIAN_POINT('Ctrl Pts',(-0.46564546202603,-1.,-1.9428979419619));
#30212=CARTESIAN_POINT('Ctrl Pts',(-0.46564546202603,1.,-1.9428979419619));
#30213=CARTESIAN_POINT('Ctrl Pts',(-0.468997482913135,-1.,-1.94794381136514));
#30214=CARTESIAN_POINT('Ctrl Pts',(-0.468997482913135,1.,-1.94794381136514));
#30215=CARTESIAN_POINT('Ctrl Pts',(-0.472397672264072,-1.,-1.95296148278133));
#30216=CARTESIAN_POINT('Ctrl Pts',(-0.472397672264072,1.,-1.95296148278133));
#30217=CARTESIAN_POINT('Ctrl Pts',(-0.475848034683176,-1.,-1.95796111148177));
#30218=CARTESIAN_POINT('Ctrl Pts',(-0.475848034683176,1.,-1.95796111148177));
#30219=CARTESIAN_POINT('Ctrl Pts',(-0.479349583074855,-1.,-1.96294933055943));
#30220=CARTESIAN_POINT('Ctrl Pts',(-0.479349583074855,1.,-1.96294933055943));
#30221=CARTESIAN_POINT('Ctrl Pts',(-0.482901662120691,-1.,-1.96792703422362));
#30222=CARTESIAN_POINT('Ctrl Pts',(-0.482901662120691,1.,-1.96792703422362));
#30223=CARTESIAN_POINT('Ctrl Pts',(-0.486502692907659,-1.,-1.97289186263272));
#30224=CARTESIAN_POINT('Ctrl Pts',(-0.486502692907659,1.,-1.97289186263272));
#30225=CARTESIAN_POINT('Ctrl Pts',(-0.490150627860952,-1.,-1.97783973019229));
#30226=CARTESIAN_POINT('Ctrl Pts',(-0.490150627860952,1.,-1.97783973019229));
#30227=CARTESIAN_POINT('Ctrl Pts',(-0.493843476541495,-1.,-1.98276658761821));
#30228=CARTESIAN_POINT('Ctrl Pts',(-0.493843476541495,1.,-1.98276658761821));
#30229=CARTESIAN_POINT('Ctrl Pts',(-0.497579909545574,-1.,-1.98767044752932));
#30230=CARTESIAN_POINT('Ctrl Pts',(-0.497579909545574,1.,-1.98767044752932));
#30231=CARTESIAN_POINT('Ctrl Pts',(-0.501359287727146,-1.,-1.99255149126155));
#30232=CARTESIAN_POINT('Ctrl Pts',(-0.501359287727146,1.,-1.99255149126155));
#30233=CARTESIAN_POINT('Ctrl Pts',(-0.505181361323026,-1.,-1.99741107463572));
#30234=CARTESIAN_POINT('Ctrl Pts',(-0.505181361323026,1.,-1.99741107463572));
#30235=CARTESIAN_POINT('Ctrl Pts',(-0.509046069886157,-1.,-2.00225107134734));
#30236=CARTESIAN_POINT('Ctrl Pts',(-0.509046069886157,1.,-2.00225107134734));
#30237=CARTESIAN_POINT('Ctrl Pts',(-0.512953306961792,-1.,-2.00707309946949));
#30238=CARTESIAN_POINT('Ctrl Pts',(-0.512953306961792,1.,-2.00707309946949));
#30239=CARTESIAN_POINT('Ctrl Pts',(-0.516902681728687,-1.,-2.01187773939242));
#30240=CARTESIAN_POINT('Ctrl Pts',(-0.516902681728687,1.,-2.01187773939242));
#30241=CARTESIAN_POINT('Ctrl Pts',(-0.52089359039937,-1.,-2.01666477917286));
#30242=CARTESIAN_POINT('Ctrl Pts',(-0.52089359039937,1.,-2.01666477917286));
#30243=CARTESIAN_POINT('Ctrl Pts',(-0.524925318333476,-1.,-2.02143356304698));
#30244=CARTESIAN_POINT('Ctrl Pts',(-0.524925318333476,1.,-2.02143356304698));
#30245=CARTESIAN_POINT('Ctrl Pts',(-0.528997127241914,-1.,-2.0261832908329));
#30246=CARTESIAN_POINT('Ctrl Pts',(-0.528997127241914,1.,-2.0261832908329));
#30247=CARTESIAN_POINT('Ctrl Pts',(-0.533108355132977,-1.,-2.03091336214426));
#30248=CARTESIAN_POINT('Ctrl Pts',(-0.533108355132977,1.,-2.03091336214426));
#30249=CARTESIAN_POINT('Ctrl Pts',(-0.537258489833262,-1.,-2.03562362954037));
#30250=CARTESIAN_POINT('Ctrl Pts',(-0.537258489833262,1.,-2.03562362954037));
#30251=CARTESIAN_POINT('Ctrl Pts',(-0.541447120615659,-1.,-2.04031422690527));
#30252=CARTESIAN_POINT('Ctrl Pts',(-0.541447120615659,1.,-2.04031422690527));
#30253=CARTESIAN_POINT('Ctrl Pts',(-0.54567390381743,-1.,-2.04498544714588));
#30254=CARTESIAN_POINT('Ctrl Pts',(-0.54567390381743,1.,-2.04498544714588));
#30255=CARTESIAN_POINT('Ctrl Pts',(-0.549938525150295,-1.,-2.04963761077958));
#30256=CARTESIAN_POINT('Ctrl Pts',(-0.549938525150295,1.,-2.04963761077958));
#30257=CARTESIAN_POINT('Ctrl Pts',(-0.554240657463906,-1.,-2.05427091604413));
#30258=CARTESIAN_POINT('Ctrl Pts',(-0.554240657463906,1.,-2.05427091604413));
#30259=CARTESIAN_POINT('Ctrl Pts',(-0.558579940185151,-1.,-2.05888537756462));
#30260=CARTESIAN_POINT('Ctrl Pts',(-0.558579940185151,1.,-2.05888537756462));
#30261=CARTESIAN_POINT('Ctrl Pts',(-0.562955993082261,-1.,-2.06348090160589));
#30262=CARTESIAN_POINT('Ctrl Pts',(-0.562955993082261,1.,-2.06348090160589));
#30263=CARTESIAN_POINT('Ctrl Pts',(-0.567368421181087,-1.,-2.06805732997334));
#30264=CARTESIAN_POINT('Ctrl Pts',(-0.567368421181087,1.,-2.06805732997334));
#30265=CARTESIAN_POINT('Ctrl Pts',(-0.571816823242603,-1.,-2.07261449292824));
#30266=CARTESIAN_POINT('Ctrl Pts',(-0.571816823242603,1.,-2.07261449292824));
#30267=CARTESIAN_POINT('Ctrl Pts',(-0.576300797416844,-1.,-2.07715226767559));
#30268=CARTESIAN_POINT('Ctrl Pts',(-0.576300797416844,1.,-2.07715226767559));
#30269=CARTESIAN_POINT('Ctrl Pts',(-0.580819952108063,-1.,-2.08167059018418));
#30270=CARTESIAN_POINT('Ctrl Pts',(-0.580819952108063,1.,-2.08167059018418));
#30271=CARTESIAN_POINT('Ctrl Pts',(-0.585373918991617,-1.,-2.08616943727951));
#30272=CARTESIAN_POINT('Ctrl Pts',(-0.585373918991617,1.,-2.08616943727951));
#30273=CARTESIAN_POINT('Ctrl Pts',(-0.589962365403406,-1.,-2.09064881812129));
#30274=CARTESIAN_POINT('Ctrl Pts',(-0.589962365403406,1.,-2.09064881812129));
#30275=CARTESIAN_POINT('Ctrl Pts',(-0.594585006052162,-1.,-2.0951087622027));
#30276=CARTESIAN_POINT('Ctrl Pts',(-0.594585006052162,1.,-2.0951087622027));
#30277=CARTESIAN_POINT('Ctrl Pts',(-0.599241616420533,-1.,-2.0995493086477));
#30278=CARTESIAN_POINT('Ctrl Pts',(-0.599241616420533,1.,-2.0995493086477));
#30279=CARTESIAN_POINT('Ctrl Pts',(-0.60393203073603,-1.,-2.10397049886949));
#30280=CARTESIAN_POINT('Ctrl Pts',(-0.60393203073603,1.,-2.10397049886949));
#30281=CARTESIAN_POINT('Ctrl Pts',(-0.607711315454876,-1.,-2.1074919961518));
#30282=CARTESIAN_POINT('Ctrl Pts',(-0.607711315454876,1.,-2.1074919961518));
#30283=CARTESIAN_POINT('Ctrl Pts',(-0.610560911689899,-1.,-2.11012443807238));
#30284=CARTESIAN_POINT('Ctrl Pts',(-0.610560911689899,1.,-2.11012443807238));
#30285=CARTESIAN_POINT('Ctrl Pts',(-0.6124673655618,-1.,-2.11187554259986));
#30286=CARTESIAN_POINT('Ctrl Pts',(-0.6124673655618,1.,-2.11187554259986));
#30287=CARTESIAN_POINT('Ctrl Pts',(-0.61342227326009,-1.,-2.11275013067528));
#30288=CARTESIAN_POINT('Ctrl Pts',(-0.61342227326009,1.,-2.11275013067528));
#30289=CARTESIAN_POINT('',(-0.383122945602004,1.,-1.7075470150345));
#30290=CARTESIAN_POINT('Ctrl Pts',(-0.383122945602004,1.,-1.7075470150345));
#30291=CARTESIAN_POINT('Ctrl Pts',(-0.384119047315542,1.,-1.71231062891958));
#30292=CARTESIAN_POINT('Ctrl Pts',(-0.38607079032701,1.,-1.72162022246158));
#30293=CARTESIAN_POINT('Ctrl Pts',(-0.388877023509191,1.,-1.7349317097561));
#30294=CARTESIAN_POINT('Ctrl Pts',(-0.392375812294307,1.,-1.75137405313962));
#30295=CARTESIAN_POINT('Ctrl Pts',(-0.39634619612042,1.,-1.7697556004756));
#30296=CARTESIAN_POINT('Ctrl Pts',(-0.39991940378308,1.,-1.78598826347533));
#30297=CARTESIAN_POINT('Ctrl Pts',(-0.403107976170441,1.,-1.80012077176221));
#30298=CARTESIAN_POINT('Ctrl Pts',(-0.405933518411838,1.,-1.81223801813988));
#30299=CARTESIAN_POINT('Ctrl Pts',(-0.408428948108533,1.,-1.8224702267854));
#30300=CARTESIAN_POINT('Ctrl Pts',(-0.410641256301675,1.,-1.83100408895216));
#30301=CARTESIAN_POINT('Ctrl Pts',(-0.412633125322162,1.,-1.83808953475839));
#30302=CARTESIAN_POINT('Ctrl Pts',(-0.41448743825434,1.,-1.8440575707371));
#30303=CARTESIAN_POINT('Ctrl Pts',(-0.416300022038864,1.,-1.84929312929882));
#30304=CARTESIAN_POINT('Ctrl Pts',(-0.418164129143534,1.,-1.85417632856234));
#30305=CARTESIAN_POINT('Ctrl Pts',(-0.420157287975619,1.,-1.85903281096686));
#30306=CARTESIAN_POINT('Ctrl Pts',(-0.422327307418275,1.,-1.86408083334028));
#30307=CARTESIAN_POINT('Ctrl Pts',(-0.424678177291359,1.,-1.86937803944323));
#30308=CARTESIAN_POINT('Ctrl Pts',(-0.427183828519102,1.,-1.87486989291484));
#30309=CARTESIAN_POINT('Ctrl Pts',(-0.429803062482344,1.,-1.88044229001832));
#30310=CARTESIAN_POINT('Ctrl Pts',(-0.432493038548748,1.,-1.88596913666793));
#30311=CARTESIAN_POINT('Ctrl Pts',(-0.435225660963383,1.,-1.89136993975504));
#30312=CARTESIAN_POINT('Ctrl Pts',(-0.437995003948244,1.,-1.89663648956466));
#30313=CARTESIAN_POINT('Ctrl Pts',(-0.440807833704038,1.,-1.90180124389086));
#30314=CARTESIAN_POINT('Ctrl Pts',(-0.443677556849151,1.,-1.90691756144898));
#30315=CARTESIAN_POINT('Ctrl Pts',(-0.446617343485711,1.,-1.9120369998112));
#30316=CARTESIAN_POINT('Ctrl Pts',(-0.449632260106662,1.,-1.91718342555755));
#30317=CARTESIAN_POINT('Ctrl Pts',(-0.452719478359432,1.,-1.92235380648502));
#30318=CARTESIAN_POINT('Ctrl Pts',(-0.455872005174371,1.,-1.92753067150476));
#30319=CARTESIAN_POINT('Ctrl Pts',(-0.459081234547926,1.,-1.93269066517934));
#30320=CARTESIAN_POINT('Ctrl Pts',(-0.462340031009056,1.,-1.93781486640821));
#30321=CARTESIAN_POINT('Ctrl Pts',(-0.46564546202603,1.,-1.9428979419619));
#30322=CARTESIAN_POINT('Ctrl Pts',(-0.468997482913135,1.,-1.94794381136514));
#30323=CARTESIAN_POINT('Ctrl Pts',(-0.472397672264072,1.,-1.95296148278133));
#30324=CARTESIAN_POINT('Ctrl Pts',(-0.475848034683176,1.,-1.95796111148177));
#30325=CARTESIAN_POINT('Ctrl Pts',(-0.479349583074855,1.,-1.96294933055943));
#30326=CARTESIAN_POINT('Ctrl Pts',(-0.482901662120691,1.,-1.96792703422362));
#30327=CARTESIAN_POINT('Ctrl Pts',(-0.486502692907659,1.,-1.97289186263272));
#30328=CARTESIAN_POINT('Ctrl Pts',(-0.490150627860952,1.,-1.97783973019229));
#30329=CARTESIAN_POINT('Ctrl Pts',(-0.493843476541495,1.,-1.98276658761821));
#30330=CARTESIAN_POINT('Ctrl Pts',(-0.497579909545574,1.,-1.98767044752932));
#30331=CARTESIAN_POINT('Ctrl Pts',(-0.501359287727146,1.,-1.99255149126155));
#30332=CARTESIAN_POINT('Ctrl Pts',(-0.505181361323026,1.,-1.99741107463572));
#30333=CARTESIAN_POINT('Ctrl Pts',(-0.509046069886157,1.,-2.00225107134734));
#30334=CARTESIAN_POINT('Ctrl Pts',(-0.512953306961792,1.,-2.00707309946949));
#30335=CARTESIAN_POINT('Ctrl Pts',(-0.516902681728687,1.,-2.01187773939242));
#30336=CARTESIAN_POINT('Ctrl Pts',(-0.52089359039937,1.,-2.01666477917286));
#30337=CARTESIAN_POINT('Ctrl Pts',(-0.524925318333476,1.,-2.02143356304698));
#30338=CARTESIAN_POINT('Ctrl Pts',(-0.528997127241914,1.,-2.0261832908329));
#30339=CARTESIAN_POINT('Ctrl Pts',(-0.533108355132977,1.,-2.03091336214426));
#30340=CARTESIAN_POINT('Ctrl Pts',(-0.537258489833262,1.,-2.03562362954037));
#30341=CARTESIAN_POINT('Ctrl Pts',(-0.541447120615659,1.,-2.04031422690527));
#30342=CARTESIAN_POINT('Ctrl Pts',(-0.54567390381743,1.,-2.04498544714588));
#30343=CARTESIAN_POINT('Ctrl Pts',(-0.549938525150295,1.,-2.04963761077958));
#30344=CARTESIAN_POINT('Ctrl Pts',(-0.554240657463906,1.,-2.05427091604413));
#30345=CARTESIAN_POINT('Ctrl Pts',(-0.558579940185151,1.,-2.05888537756462));
#30346=CARTESIAN_POINT('Ctrl Pts',(-0.562955993082261,1.,-2.06348090160589));
#30347=CARTESIAN_POINT('Ctrl Pts',(-0.567368421181087,1.,-2.06805732997334));
#30348=CARTESIAN_POINT('Ctrl Pts',(-0.571816823242603,1.,-2.07261449292824));
#30349=CARTESIAN_POINT('Ctrl Pts',(-0.576300797416844,1.,-2.07715226767559));
#30350=CARTESIAN_POINT('Ctrl Pts',(-0.580819952108063,1.,-2.08167059018418));
#30351=CARTESIAN_POINT('Ctrl Pts',(-0.585373918991617,1.,-2.08616943727951));
#30352=CARTESIAN_POINT('Ctrl Pts',(-0.589962365403406,1.,-2.09064881812129));
#30353=CARTESIAN_POINT('Ctrl Pts',(-0.594585006052162,1.,-2.0951087622027));
#30354=CARTESIAN_POINT('Ctrl Pts',(-0.599241616420533,1.,-2.0995493086477));
#30355=CARTESIAN_POINT('Ctrl Pts',(-0.60393203073603,1.,-2.10397049886949));
#30356=CARTESIAN_POINT('Ctrl Pts',(-0.607711315454876,1.,-2.1074919961518));
#30357=CARTESIAN_POINT('Ctrl Pts',(-0.610560911689899,1.,-2.11012443807238));
#30358=CARTESIAN_POINT('Ctrl Pts',(-0.6124673655618,1.,-2.11187554259986));
#30359=CARTESIAN_POINT('Ctrl Pts',(-0.61342227326009,1.,-2.11275013067528));
#30360=CARTESIAN_POINT('',(-0.383122945602003,0.,-1.7075470150345));
#30361=CARTESIAN_POINT('Origin',(0.,0.,0.));
#30362=CARTESIAN_POINT('',(-0.163289472382896,1.,-1.74236521665491));
#30363=CARTESIAN_POINT('Origin',(0.,1.,0.));
#30364=CARTESIAN_POINT('',(-0.163289472382896,0.,-1.74236521665491));
#30365=CARTESIAN_POINT('Ctrl Pts',(-0.0694764450219581,-1.,-2.19890268624765));
#30366=CARTESIAN_POINT('Ctrl Pts',(-0.0694764450219581,1.,-2.19890268624765));
#30367=CARTESIAN_POINT('Ctrl Pts',(-0.070114353632549,-1.,-2.19777582085423));
#30368=CARTESIAN_POINT('Ctrl Pts',(-0.070114353632549,1.,-2.19777582085423));
#30369=CARTESIAN_POINT('Ctrl Pts',(-0.0713863779526154,-1.,-2.19552129484002));
#30370=CARTESIAN_POINT('Ctrl Pts',(-0.0713863779526154,1.,-2.19552129484002));
#30371=CARTESIAN_POINT('Ctrl Pts',(-0.0732830357306725,-1.,-2.19213712013662));
#30372=CARTESIAN_POINT('Ctrl Pts',(-0.0732830357306725,1.,-2.19213712013662));
#30373=CARTESIAN_POINT('Ctrl Pts',(-0.0757891465836148,-1.,-2.1876201139953));
#30374=CARTESIAN_POINT('Ctrl Pts',(-0.0757891465836148,1.,-2.1876201139953));
#30375=CARTESIAN_POINT('Ctrl Pts',(-0.0788837727685243,-1.,-2.18196589448887));
#30376=CARTESIAN_POINT('Ctrl Pts',(-0.0788837727685243,1.,-2.18196589448887));
#30377=CARTESIAN_POINT('Ctrl Pts',(-0.0819402680872765,-1.,-2.176303712113));
#30378=CARTESIAN_POINT('Ctrl Pts',(-0.0819402680872765,1.,-2.176303712113));
#30379=CARTESIAN_POINT('Ctrl Pts',(-0.0849584620835372,-1.,-2.17063357870952));
#30380=CARTESIAN_POINT('Ctrl Pts',(-0.0849584620835372,1.,-2.17063357870952));
#30381=CARTESIAN_POINT('Ctrl Pts',(-0.0879381291386923,-1.,-2.16495552645014));
#30382=CARTESIAN_POINT('Ctrl Pts',(-0.0879381291386923,1.,-2.16495552645014));
#30383=CARTESIAN_POINT('Ctrl Pts',(-0.0908789888107265,-1.,-2.15926961544516));
#30384=CARTESIAN_POINT('Ctrl Pts',(-0.0908789888107265,1.,-2.15926961544516));
#30385=CARTESIAN_POINT('Ctrl Pts',(-0.0937807218867643,-1.,-2.1535759397817));
#30386=CARTESIAN_POINT('Ctrl Pts',(-0.0937807218867643,1.,-2.1535759397817));
#30387=CARTESIAN_POINT('Ctrl Pts',(-0.0966429852305459,-1.,-2.14787463531795));
#30388=CARTESIAN_POINT('Ctrl Pts',(-0.0966429852305459,1.,-2.14787463531795));
#30389=CARTESIAN_POINT('Ctrl Pts',(-0.0994654261990915,-1.,-2.14216588396025));
#30390=CARTESIAN_POINT('Ctrl Pts',(-0.0994654261990915,1.,-2.14216588396025));
#30391=CARTESIAN_POINT('Ctrl Pts',(-0.1022477005561,-1.,-2.13644992667165));
#30392=CARTESIAN_POINT('Ctrl Pts',(-0.1022477005561,1.,-2.13644992667165));
#30393=CARTESIAN_POINT('Ctrl Pts',(-0.104989479152739,-1.,-2.13072704887293));
#30394=CARTESIAN_POINT('Ctrl Pts',(-0.104989479152739,1.,-2.13072704887293));
#30395=CARTESIAN_POINT('Ctrl Pts',(-0.10769043523109,-1.,-2.12499752307));
#30396=CARTESIAN_POINT('Ctrl Pts',(-0.10769043523109,1.,-2.12499752307));
#30397=CARTESIAN_POINT('Ctrl Pts',(-0.110350236135025,-1.,-2.11926155590865));
#30398=CARTESIAN_POINT('Ctrl Pts',(-0.110350236135025,1.,-2.11926155590865));
#30399=CARTESIAN_POINT('Ctrl Pts',(-0.112968534419737,-1.,-2.11351924490306));
#30400=CARTESIAN_POINT('Ctrl Pts',(-0.112968534419737,1.,-2.11351924490306));
#30401=CARTESIAN_POINT('Ctrl Pts',(-0.115544957687926,-1.,-2.10777050261309));
#30402=CARTESIAN_POINT('Ctrl Pts',(-0.115544957687926,1.,-2.10777050261309));
#30403=CARTESIAN_POINT('Ctrl Pts',(-0.118079107988355,-1.,-2.102015121329));
#30404=CARTESIAN_POINT('Ctrl Pts',(-0.118079107988355,1.,-2.102015121329));
#30405=CARTESIAN_POINT('Ctrl Pts',(-0.120570567965122,-1.,-2.0962529286773));
#30406=CARTESIAN_POINT('Ctrl Pts',(-0.120570567965122,1.,-2.0962529286773));
#30407=CARTESIAN_POINT('Ctrl Pts',(-0.123018905621083,-1.,-2.09048392424825));
#30408=CARTESIAN_POINT('Ctrl Pts',(-0.123018905621083,1.,-2.09048392424825));
#30409=CARTESIAN_POINT('Ctrl Pts',(-0.125423679412061,-1.,-2.08470840653643));
#30410=CARTESIAN_POINT('Ctrl Pts',(-0.125423679412061,1.,-2.08470840653643));
#30411=CARTESIAN_POINT('Ctrl Pts',(-0.12778444527612,-1.,-2.07892715110987));
#30412=CARTESIAN_POINT('Ctrl Pts',(-0.12778444527612,1.,-2.07892715110987));
#30413=CARTESIAN_POINT('Ctrl Pts',(-0.130100748328403,-1.,-2.07314114713063));
#30414=CARTESIAN_POINT('Ctrl Pts',(-0.130100748328403,1.,-2.07314114713063));
#30415=CARTESIAN_POINT('Ctrl Pts',(-0.13237211154771,-1.,-2.06735123910326));
#30416=CARTESIAN_POINT('Ctrl Pts',(-0.13237211154771,1.,-2.06735123910326));
#30417=CARTESIAN_POINT('Ctrl Pts',(-0.134598026192106,-1.,-2.06155781517842));
#30418=CARTESIAN_POINT('Ctrl Pts',(-0.134598026192106,1.,-2.06155781517842));
#30419=CARTESIAN_POINT('Ctrl Pts',(-0.136777941218044,-1.,-2.05576044414264));
#30420=CARTESIAN_POINT('Ctrl Pts',(-0.136777941218044,1.,-2.05576044414264));
#30421=CARTESIAN_POINT('Ctrl Pts',(-0.138911255368966,-1.,-2.04995762001328));
#30422=CARTESIAN_POINT('Ctrl Pts',(-0.138911255368966,1.,-2.04995762001328));
#30423=CARTESIAN_POINT('Ctrl Pts',(-0.140997332152546,-1.,-2.04414757947916));
#30424=CARTESIAN_POINT('Ctrl Pts',(-0.140997332152546,1.,-2.04414757947916));
#30425=CARTESIAN_POINT('Ctrl Pts',(-0.143035515058209,-1.,-2.03832911025912));
#30426=CARTESIAN_POINT('Ctrl Pts',(-0.143035515058209,1.,-2.03832911025912));
#30427=CARTESIAN_POINT('Ctrl Pts',(-0.145025140186057,-1.,-2.03250223739942));
#30428=CARTESIAN_POINT('Ctrl Pts',(-0.145025140186057,1.,-2.03250223739942));
#30429=CARTESIAN_POINT('Ctrl Pts',(-0.146965557332583,-1.,-2.02666926182017));
#30430=CARTESIAN_POINT('Ctrl Pts',(-0.146965557332583,1.,-2.02666926182017));
#30431=CARTESIAN_POINT('Ctrl Pts',(-0.148856124775337,-1.,-2.02083464969894));
#30432=CARTESIAN_POINT('Ctrl Pts',(-0.148856124775337,1.,-2.02083464969894));
#30433=CARTESIAN_POINT('Ctrl Pts',(-0.150696157673078,-1.,-2.01500291940238));
#30434=CARTESIAN_POINT('Ctrl Pts',(-0.150696157673078,1.,-2.01500291940238));
#30435=CARTESIAN_POINT('Ctrl Pts',(-0.15248488362145,-1.,-2.00917680318424));
#30436=CARTESIAN_POINT('Ctrl Pts',(-0.15248488362145,1.,-2.00917680318424));
#30437=CARTESIAN_POINT('Ctrl Pts',(-0.154221403049722,-1.,-2.00335565310543));
#30438=CARTESIAN_POINT('Ctrl Pts',(-0.154221403049722,1.,-2.00335565310543));
#30439=CARTESIAN_POINT('Ctrl Pts',(-0.155904629548783,-1.,-1.99753284771497));
#30440=CARTESIAN_POINT('Ctrl Pts',(-0.155904629548783,1.,-1.99753284771497));
#30441=CARTESIAN_POINT('Ctrl Pts',(-0.157533331459227,-1.,-1.99169810931908));
#30442=CARTESIAN_POINT('Ctrl Pts',(-0.157533331459227,1.,-1.99169810931908));
#30443=CARTESIAN_POINT('Ctrl Pts',(-0.159106226437299,-1.,-1.98584238283292));
#30444=CARTESIAN_POINT('Ctrl Pts',(-0.159106226437299,1.,-1.98584238283292));
#30445=CARTESIAN_POINT('Ctrl Pts',(-0.160622060784611,-1.,-1.97996195437559));
#30446=CARTESIAN_POINT('Ctrl Pts',(-0.160622060784611,1.,-1.97996195437559));
#30447=CARTESIAN_POINT('Ctrl Pts',(-0.162079693556289,-1.,-1.97406280235188));
#30448=CARTESIAN_POINT('Ctrl Pts',(-0.162079693556289,1.,-1.97406280235188));
#30449=CARTESIAN_POINT('Ctrl Pts',(-0.163478185457734,-1.,-1.96816512677967));
#30450=CARTESIAN_POINT('Ctrl Pts',(-0.163478185457734,1.,-1.96816512677967));
#30451=CARTESIAN_POINT('Ctrl Pts',(-0.164816568920269,-1.,-1.96229379940136));
#30452=CARTESIAN_POINT('Ctrl Pts',(-0.164816568920269,1.,-1.96229379940136));
#30453=CARTESIAN_POINT('Ctrl Pts',(-0.166093592002812,-1.,-1.9564675971873));
#30454=CARTESIAN_POINT('Ctrl Pts',(-0.166093592002812,1.,-1.9564675971873));
#30455=CARTESIAN_POINT('Ctrl Pts',(-0.167307501784475,-1.,-1.95069027794294));
#30456=CARTESIAN_POINT('Ctrl Pts',(-0.167307501784475,1.,-1.95069027794294));
#30457=CARTESIAN_POINT('Ctrl Pts',(-0.168455741607556,-1.,-1.94493757756931));
#30458=CARTESIAN_POINT('Ctrl Pts',(-0.168455741607556,1.,-1.94493757756931));
#30459=CARTESIAN_POINT('Ctrl Pts',(-0.169534904817491,-1.,-1.93915639211581));
#30460=CARTESIAN_POINT('Ctrl Pts',(-0.169534904817491,1.,-1.93915639211581));
#30461=CARTESIAN_POINT('Ctrl Pts',(-0.170541253116202,-1.,-1.93329183155539));
#30462=CARTESIAN_POINT('Ctrl Pts',(-0.170541253116202,1.,-1.93329183155539));
#30463=CARTESIAN_POINT('Ctrl Pts',(-0.171471191532988,-1.,-1.92731093582036));
#30464=CARTESIAN_POINT('Ctrl Pts',(-0.171471191532988,1.,-1.92731093582036));
#30465=CARTESIAN_POINT('Ctrl Pts',(-0.172321621259514,-1.,-1.9212233439798));
#30466=CARTESIAN_POINT('Ctrl Pts',(-0.172321621259514,1.,-1.9212233439798));
#30467=CARTESIAN_POINT('Ctrl Pts',(-0.173090695383496,-1.,-1.91511429159527));
#30468=CARTESIAN_POINT('Ctrl Pts',(-0.173090695383496,1.,-1.91511429159527));
#30469=CARTESIAN_POINT('Ctrl Pts',(-0.173776635257817,-1.,-1.90911693975267));
#30470=CARTESIAN_POINT('Ctrl Pts',(-0.173776635257817,1.,-1.90911693975267));
#30471=CARTESIAN_POINT('Ctrl Pts',(-0.174375518661085,-1.,-1.90335253862834));
#30472=CARTESIAN_POINT('Ctrl Pts',(-0.174375518661085,1.,-1.90335253862834));
#30473=CARTESIAN_POINT('Ctrl Pts',(-0.174879405091263,-1.,-1.89788101117132));
#30474=CARTESIAN_POINT('Ctrl Pts',(-0.174879405091263,1.,-1.89788101117132));
#30475=CARTESIAN_POINT('Ctrl Pts',(-0.175274276190844,-1.,-1.892646301985));
#30476=CARTESIAN_POINT('Ctrl Pts',(-0.175274276190844,1.,-1.892646301985));
#30477=CARTESIAN_POINT('Ctrl Pts',(-0.175538155840648,-1.,-1.88742606273259));
#30478=CARTESIAN_POINT('Ctrl Pts',(-0.175538155840648,1.,-1.88742606273259));
#30479=CARTESIAN_POINT('Ctrl Pts',(-0.175644148889699,-1.,-1.88188663145367));
#30480=CARTESIAN_POINT('Ctrl Pts',(-0.175644148889699,1.,-1.88188663145367));
#30481=CARTESIAN_POINT('Ctrl Pts',(-0.175563480746485,-1.,-1.87563767773588));
#30482=CARTESIAN_POINT('Ctrl Pts',(-0.175563480746485,1.,-1.87563767773588));
#30483=CARTESIAN_POINT('Ctrl Pts',(-0.175268337590758,-1.,-1.86828349694799));
#30484=CARTESIAN_POINT('Ctrl Pts',(-0.175268337590758,1.,-1.86828349694799));
#30485=CARTESIAN_POINT('Ctrl Pts',(-0.17473525927603,-1.,-1.85948367088837));
#30486=CARTESIAN_POINT('Ctrl Pts',(-0.17473525927603,1.,-1.85948367088837));
#30487=CARTESIAN_POINT('Ctrl Pts',(-0.173946627587731,-1.,-1.8489811319852));
#30488=CARTESIAN_POINT('Ctrl Pts',(-0.173946627587731,1.,-1.8489811319852));
#30489=CARTESIAN_POINT('Ctrl Pts',(-0.1728894428919,-1.,-1.83658380527692));
#30490=CARTESIAN_POINT('Ctrl Pts',(-0.1728894428919,1.,-1.83658380527692));
#30491=CARTESIAN_POINT('Ctrl Pts',(-0.171554770204119,-1.,-1.82215766811545));
#30492=CARTESIAN_POINT('Ctrl Pts',(-0.171554770204119,1.,-1.82215766811545));
#30493=CARTESIAN_POINT('Ctrl Pts',(-0.169936923904608,-1.,-1.80561530629706));
#30494=CARTESIAN_POINT('Ctrl Pts',(-0.169936923904608,1.,-1.80561530629706));
#30495=CARTESIAN_POINT('Ctrl Pts',(-0.168032772805197,-1.,-1.7869064998507));
#30496=CARTESIAN_POINT('Ctrl Pts',(-0.168032772805197,1.,-1.7869064998507));
#30497=CARTESIAN_POINT('Ctrl Pts',(-0.1662793551464,-1.,-1.77018771684844));
#30498=CARTESIAN_POINT('Ctrl Pts',(-0.1662793551464,1.,-1.77018771684844));
#30499=CARTESIAN_POINT('Ctrl Pts',(-0.164834765707158,-1.,-1.75666056638427));
#30500=CARTESIAN_POINT('Ctrl Pts',(-0.164834765707158,1.,-1.75666056638427));
#30501=CARTESIAN_POINT('Ctrl Pts',(-0.163814161002002,-1.,-1.7472034950333));
#30502=CARTESIAN_POINT('Ctrl Pts',(-0.163814161002002,1.,-1.7472034950333));
#30503=CARTESIAN_POINT('Ctrl Pts',(-0.163289472382896,-1.,-1.74236521665491));
#30504=CARTESIAN_POINT('Ctrl Pts',(-0.163289472382896,1.,-1.74236521665491));
#30505=CARTESIAN_POINT('',(-0.0694764450219581,1.,-2.19890268624765));
#30506=CARTESIAN_POINT('Ctrl Pts',(-0.0694764450219581,1.,-2.19890268624765));
#30507=CARTESIAN_POINT('Ctrl Pts',(-0.070114353632549,1.,-2.19777582085423));
#30508=CARTESIAN_POINT('Ctrl Pts',(-0.0713863779526154,1.,-2.19552129484002));
#30509=CARTESIAN_POINT('Ctrl Pts',(-0.0732830357306725,1.,-2.19213712013662));
#30510=CARTESIAN_POINT('Ctrl Pts',(-0.0757891465836148,1.,-2.1876201139953));
#30511=CARTESIAN_POINT('Ctrl Pts',(-0.0788837727685243,1.,-2.18196589448887));
#30512=CARTESIAN_POINT('Ctrl Pts',(-0.0819402680872765,1.,-2.176303712113));
#30513=CARTESIAN_POINT('Ctrl Pts',(-0.0849584620835372,1.,-2.17063357870952));
#30514=CARTESIAN_POINT('Ctrl Pts',(-0.0879381291386923,1.,-2.16495552645014));
#30515=CARTESIAN_POINT('Ctrl Pts',(-0.0908789888107265,1.,-2.15926961544516));
#30516=CARTESIAN_POINT('Ctrl Pts',(-0.0937807218867643,1.,-2.1535759397817));
#30517=CARTESIAN_POINT('Ctrl Pts',(-0.0966429852305459,1.,-2.14787463531795));
#30518=CARTESIAN_POINT('Ctrl Pts',(-0.0994654261990915,1.,-2.14216588396025));
#30519=CARTESIAN_POINT('Ctrl Pts',(-0.1022477005561,1.,-2.13644992667165));
#30520=CARTESIAN_POINT('Ctrl Pts',(-0.104989479152739,1.,-2.13072704887293));
#30521=CARTESIAN_POINT('Ctrl Pts',(-0.10769043523109,1.,-2.12499752307));
#30522=CARTESIAN_POINT('Ctrl Pts',(-0.110350236135025,1.,-2.11926155590865));
#30523=CARTESIAN_POINT('Ctrl Pts',(-0.112968534419737,1.,-2.11351924490306));
#30524=CARTESIAN_POINT('Ctrl Pts',(-0.115544957687926,1.,-2.10777050261309));
#30525=CARTESIAN_POINT('Ctrl Pts',(-0.118079107988355,1.,-2.102015121329));
#30526=CARTESIAN_POINT('Ctrl Pts',(-0.120570567965122,1.,-2.0962529286773));
#30527=CARTESIAN_POINT('Ctrl Pts',(-0.123018905621083,1.,-2.09048392424825));
#30528=CARTESIAN_POINT('Ctrl Pts',(-0.125423679412061,1.,-2.08470840653643));
#30529=CARTESIAN_POINT('Ctrl Pts',(-0.12778444527612,1.,-2.07892715110987));
#30530=CARTESIAN_POINT('Ctrl Pts',(-0.130100748328403,1.,-2.07314114713063));
#30531=CARTESIAN_POINT('Ctrl Pts',(-0.13237211154771,1.,-2.06735123910326));
#30532=CARTESIAN_POINT('Ctrl Pts',(-0.134598026192106,1.,-2.06155781517842));
#30533=CARTESIAN_POINT('Ctrl Pts',(-0.136777941218044,1.,-2.05576044414264));
#30534=CARTESIAN_POINT('Ctrl Pts',(-0.138911255368966,1.,-2.04995762001328));
#30535=CARTESIAN_POINT('Ctrl Pts',(-0.140997332152546,1.,-2.04414757947916));
#30536=CARTESIAN_POINT('Ctrl Pts',(-0.143035515058209,1.,-2.03832911025912));
#30537=CARTESIAN_POINT('Ctrl Pts',(-0.145025140186057,1.,-2.03250223739942));
#30538=CARTESIAN_POINT('Ctrl Pts',(-0.146965557332583,1.,-2.02666926182017));
#30539=CARTESIAN_POINT('Ctrl Pts',(-0.148856124775337,1.,-2.02083464969894));
#30540=CARTESIAN_POINT('Ctrl Pts',(-0.150696157673078,1.,-2.01500291940238));
#30541=CARTESIAN_POINT('Ctrl Pts',(-0.15248488362145,1.,-2.00917680318424));
#30542=CARTESIAN_POINT('Ctrl Pts',(-0.154221403049722,1.,-2.00335565310543));
#30543=CARTESIAN_POINT('Ctrl Pts',(-0.155904629548783,1.,-1.99753284771497));
#30544=CARTESIAN_POINT('Ctrl Pts',(-0.157533331459227,1.,-1.99169810931908));
#30545=CARTESIAN_POINT('Ctrl Pts',(-0.159106226437299,1.,-1.98584238283292));
#30546=CARTESIAN_POINT('Ctrl Pts',(-0.160622060784611,1.,-1.97996195437559));
#30547=CARTESIAN_POINT('Ctrl Pts',(-0.162079693556289,1.,-1.97406280235188));
#30548=CARTESIAN_POINT('Ctrl Pts',(-0.163478185457734,1.,-1.96816512677967));
#30549=CARTESIAN_POINT('Ctrl Pts',(-0.164816568920269,1.,-1.96229379940136));
#30550=CARTESIAN_POINT('Ctrl Pts',(-0.166093592002812,1.,-1.9564675971873));
#30551=CARTESIAN_POINT('Ctrl Pts',(-0.167307501784475,1.,-1.95069027794294));
#30552=CARTESIAN_POINT('Ctrl Pts',(-0.168455741607556,1.,-1.94493757756931));
#30553=CARTESIAN_POINT('Ctrl Pts',(-0.169534904817491,1.,-1.93915639211581));
#30554=CARTESIAN_POINT('Ctrl Pts',(-0.170541253116202,1.,-1.93329183155539));
#30555=CARTESIAN_POINT('Ctrl Pts',(-0.171471191532988,1.,-1.92731093582036));
#30556=CARTESIAN_POINT('Ctrl Pts',(-0.172321621259514,1.,-1.9212233439798));
#30557=CARTESIAN_POINT('Ctrl Pts',(-0.173090695383496,1.,-1.91511429159527));
#30558=CARTESIAN_POINT('Ctrl Pts',(-0.173776635257817,1.,-1.90911693975267));
#30559=CARTESIAN_POINT('Ctrl Pts',(-0.174375518661085,1.,-1.90335253862834));
#30560=CARTESIAN_POINT('Ctrl Pts',(-0.174879405091263,1.,-1.89788101117132));
#30561=CARTESIAN_POINT('Ctrl Pts',(-0.175274276190844,1.,-1.892646301985));
#30562=CARTESIAN_POINT('Ctrl Pts',(-0.175538155840648,1.,-1.88742606273259));
#30563=CARTESIAN_POINT('Ctrl Pts',(-0.175644148889699,1.,-1.88188663145367));
#30564=CARTESIAN_POINT('Ctrl Pts',(-0.175563480746485,1.,-1.87563767773588));
#30565=CARTESIAN_POINT('Ctrl Pts',(-0.175268337590758,1.,-1.86828349694799));
#30566=CARTESIAN_POINT('Ctrl Pts',(-0.17473525927603,1.,-1.85948367088837));
#30567=CARTESIAN_POINT('Ctrl Pts',(-0.173946627587731,1.,-1.8489811319852));
#30568=CARTESIAN_POINT('Ctrl Pts',(-0.1728894428919,1.,-1.83658380527692));
#30569=CARTESIAN_POINT('Ctrl Pts',(-0.171554770204119,1.,-1.82215766811545));
#30570=CARTESIAN_POINT('Ctrl Pts',(-0.169936923904608,1.,-1.80561530629706));
#30571=CARTESIAN_POINT('Ctrl Pts',(-0.168032772805197,1.,-1.7869064998507));
#30572=CARTESIAN_POINT('Ctrl Pts',(-0.1662793551464,1.,-1.77018771684844));
#30573=CARTESIAN_POINT('Ctrl Pts',(-0.164834765707158,1.,-1.75666056638427));
#30574=CARTESIAN_POINT('Ctrl Pts',(-0.163814161002002,1.,-1.7472034950333));
#30575=CARTESIAN_POINT('Ctrl Pts',(-0.163289472382896,1.,-1.74236521665491));
#30576=CARTESIAN_POINT('',(-0.0694764450219581,0.,-2.19890268624765));
#30577=CARTESIAN_POINT('Origin',(0.0694764450219584,0.,-2.19890268624765));
#30578=CARTESIAN_POINT('',(0.0694764450219584,1.,-2.19890268624765));
#30579=CARTESIAN_POINT('',(-0.0694764450219581,1.,-2.19890268624765));
#30580=CARTESIAN_POINT('',(0.0694764450219584,0.,-2.19890268624765));
#30581=CARTESIAN_POINT('Ctrl Pts',(0.163289472382896,-1.,-1.74236521665491));
#30582=CARTESIAN_POINT('Ctrl Pts',(0.163289472382896,1.,-1.74236521665491));
#30583=CARTESIAN_POINT('Ctrl Pts',(0.163814161002474,-1.,-1.74720349503904));
#30584=CARTESIAN_POINT('Ctrl Pts',(0.163814161002474,1.,-1.74720349503904));
#30585=CARTESIAN_POINT('Ctrl Pts',(0.164834765708484,-1.,-1.75666056640041));
#30586=CARTESIAN_POINT('Ctrl Pts',(0.164834765708484,1.,-1.75666056640041));
#30587=CARTESIAN_POINT('Ctrl Pts',(0.166279355148738,-1.,-1.77018771687692));
#30588=CARTESIAN_POINT('Ctrl Pts',(0.166279355148738,1.,-1.77018771687692));
#30589=CARTESIAN_POINT('Ctrl Pts',(0.16803277280837,-1.,-1.78690649988931));
#30590=CARTESIAN_POINT('Ctrl Pts',(0.16803277280837,1.,-1.78690649988931));
#30591=CARTESIAN_POINT('Ctrl Pts',(0.169936923908078,-1.,-1.80561530633924));
#30592=CARTESIAN_POINT('Ctrl Pts',(0.169936923908078,1.,-1.80561530633924));
#30593=CARTESIAN_POINT('Ctrl Pts',(0.171554770207306,-1.,-1.82215766815414));
#30594=CARTESIAN_POINT('Ctrl Pts',(0.171554770207306,1.,-1.82215766815414));
#30595=CARTESIAN_POINT('Ctrl Pts',(0.17288944289442,-1.,-1.83658380530747));
#30596=CARTESIAN_POINT('Ctrl Pts',(0.17288944289442,1.,-1.83658380530747));
#30597=CARTESIAN_POINT('Ctrl Pts',(0.173946627589401,-1.,-1.84898113200543));
#30598=CARTESIAN_POINT('Ctrl Pts',(0.173946627589401,1.,-1.84898113200543));
#30599=CARTESIAN_POINT('Ctrl Pts',(0.174735259276856,-1.,-1.85948367089838));
#30600=CARTESIAN_POINT('Ctrl Pts',(0.174735259276856,1.,-1.85948367089838));
#30601=CARTESIAN_POINT('Ctrl Pts',(0.175268337590901,-1.,-1.86828349694972));
#30602=CARTESIAN_POINT('Ctrl Pts',(0.175268337590901,1.,-1.86828349694972));
#30603=CARTESIAN_POINT('Ctrl Pts',(0.175563480746205,-1.,-1.87563767773249));
#30604=CARTESIAN_POINT('Ctrl Pts',(0.175563480746205,1.,-1.87563767773249));
#30605=CARTESIAN_POINT('Ctrl Pts',(0.175644148889271,-1.,-1.88188663144846));
#30606=CARTESIAN_POINT('Ctrl Pts',(0.175644148889271,1.,-1.88188663144846));
#30607=CARTESIAN_POINT('Ctrl Pts',(0.175538155840286,-1.,-1.88742606272818));
#30608=CARTESIAN_POINT('Ctrl Pts',(0.175538155840286,1.,-1.88742606272818));
#30609=CARTESIAN_POINT('Ctrl Pts',(0.175274276190664,-1.,-1.89264630198279));
#30610=CARTESIAN_POINT('Ctrl Pts',(0.175274276190664,1.,-1.89264630198279));
#30611=CARTESIAN_POINT('Ctrl Pts',(0.174879405091277,-1.,-1.89788101117148));
#30612=CARTESIAN_POINT('Ctrl Pts',(0.174879405091277,1.,-1.89788101117148));
#30613=CARTESIAN_POINT('Ctrl Pts',(0.174375518661222,-1.,-1.90335253863003));
#30614=CARTESIAN_POINT('Ctrl Pts',(0.174375518661222,1.,-1.90335253863003));
#30615=CARTESIAN_POINT('Ctrl Pts',(0.173776635257984,-1.,-1.90911693975475));
#30616=CARTESIAN_POINT('Ctrl Pts',(0.173776635257984,1.,-1.90911693975475));
#30617=CARTESIAN_POINT('Ctrl Pts',(0.173090695383619,-1.,-1.91511429159681));
#30618=CARTESIAN_POINT('Ctrl Pts',(0.173090695383619,1.,-1.91511429159681));
#30619=CARTESIAN_POINT('Ctrl Pts',(0.172321621259557,-1.,-1.92122334398034));
#30620=CARTESIAN_POINT('Ctrl Pts',(0.172321621259557,1.,-1.92122334398034));
#30621=CARTESIAN_POINT('Ctrl Pts',(0.17147119153296,-1.,-1.92731093582));
#30622=CARTESIAN_POINT('Ctrl Pts',(0.17147119153296,1.,-1.92731093582));
#30623=CARTESIAN_POINT('Ctrl Pts',(0.170541253116136,-1.,-1.93329183155455));
#30624=CARTESIAN_POINT('Ctrl Pts',(0.170541253116136,1.,-1.93329183155455));
#30625=CARTESIAN_POINT('Ctrl Pts',(0.169534904817425,-1.,-1.93915639211497));
#30626=CARTESIAN_POINT('Ctrl Pts',(0.169534904817425,1.,-1.93915639211497));
#30627=CARTESIAN_POINT('Ctrl Pts',(0.168455741607516,-1.,-1.94493757756879));
#30628=CARTESIAN_POINT('Ctrl Pts',(0.168455741607516,1.,-1.94493757756879));
#30629=CARTESIAN_POINT('Ctrl Pts',(0.167307501784469,-1.,-1.95069027794286));
#30630=CARTESIAN_POINT('Ctrl Pts',(0.167307501784469,1.,-1.95069027794286));
#30631=CARTESIAN_POINT('Ctrl Pts',(0.166093592002833,-1.,-1.95646759718755));
#30632=CARTESIAN_POINT('Ctrl Pts',(0.166093592002833,1.,-1.95646759718755));
#30633=CARTESIAN_POINT('Ctrl Pts',(0.1648165689203,-1.,-1.96229379940174));
#30634=CARTESIAN_POINT('Ctrl Pts',(0.1648165689203,1.,-1.96229379940174));
#30635=CARTESIAN_POINT('Ctrl Pts',(0.16347818545776,-1.,-1.96816512678));
#30636=CARTESIAN_POINT('Ctrl Pts',(0.16347818545776,1.,-1.96816512678));
#30637=CARTESIAN_POINT('Ctrl Pts',(0.162079693556302,-1.,-1.97406280235204));
#30638=CARTESIAN_POINT('Ctrl Pts',(0.162079693556302,1.,-1.97406280235204));
#30639=CARTESIAN_POINT('Ctrl Pts',(0.16062206078461,-1.,-1.97996195437557));
#30640=CARTESIAN_POINT('Ctrl Pts',(0.16062206078461,1.,-1.97996195437557));
#30641=CARTESIAN_POINT('Ctrl Pts',(0.159106226437288,-1.,-1.98584238283279));
#30642=CARTESIAN_POINT('Ctrl Pts',(0.159106226437288,1.,-1.98584238283279));
#30643=CARTESIAN_POINT('Ctrl Pts',(0.157533331459215,-1.,-1.99169810931893));
#30644=CARTESIAN_POINT('Ctrl Pts',(0.157533331459215,1.,-1.99169810931893));
#30645=CARTESIAN_POINT('Ctrl Pts',(0.155904629548774,-1.,-1.99753284771487));
#30646=CARTESIAN_POINT('Ctrl Pts',(0.155904629548774,1.,-1.99753284771487));
#30647=CARTESIAN_POINT('Ctrl Pts',(0.154221403049719,-1.,-2.00335565310539));
#30648=CARTESIAN_POINT('Ctrl Pts',(0.154221403049719,1.,-2.00335565310539));
#30649=CARTESIAN_POINT('Ctrl Pts',(0.152484883621452,-1.,-2.00917680318426));
#30650=CARTESIAN_POINT('Ctrl Pts',(0.152484883621452,1.,-2.00917680318426));
#30651=CARTESIAN_POINT('Ctrl Pts',(0.150696157673084,-1.,-2.01500291940243));
#30652=CARTESIAN_POINT('Ctrl Pts',(0.150696157673084,1.,-2.01500291940243));
#30653=CARTESIAN_POINT('Ctrl Pts',(0.148856124775343,-1.,-2.02083464969897));
#30654=CARTESIAN_POINT('Ctrl Pts',(0.148856124775343,1.,-2.02083464969897));
#30655=CARTESIAN_POINT('Ctrl Pts',(0.146965557332586,-1.,-2.02666926182017));
#30656=CARTESIAN_POINT('Ctrl Pts',(0.146965557332586,1.,-2.02666926182017));
#30657=CARTESIAN_POINT('Ctrl Pts',(0.145025140186058,-1.,-2.03250223739941));
#30658=CARTESIAN_POINT('Ctrl Pts',(0.145025140186058,1.,-2.03250223739941));
#30659=CARTESIAN_POINT('Ctrl Pts',(0.143035515058208,-1.,-2.03832911025913));
#30660=CARTESIAN_POINT('Ctrl Pts',(0.143035515058208,1.,-2.03832911025913));
#30661=CARTESIAN_POINT('Ctrl Pts',(0.140997332152545,-1.,-2.04414757947919));
#30662=CARTESIAN_POINT('Ctrl Pts',(0.140997332152545,1.,-2.04414757947919));
#30663=CARTESIAN_POINT('Ctrl Pts',(0.138911255368966,-1.,-2.04995762001333));
#30664=CARTESIAN_POINT('Ctrl Pts',(0.138911255368966,1.,-2.04995762001333));
#30665=CARTESIAN_POINT('Ctrl Pts',(0.136777941218044,-1.,-2.0557604441427));
#30666=CARTESIAN_POINT('Ctrl Pts',(0.136777941218044,1.,-2.0557604441427));
#30667=CARTESIAN_POINT('Ctrl Pts',(0.134598026192107,-1.,-2.06155781517844));
#30668=CARTESIAN_POINT('Ctrl Pts',(0.134598026192107,1.,-2.06155781517844));
#30669=CARTESIAN_POINT('Ctrl Pts',(0.13237211154771,-1.,-2.06735123910319));
#30670=CARTESIAN_POINT('Ctrl Pts',(0.13237211154771,1.,-2.06735123910319));
#30671=CARTESIAN_POINT('Ctrl Pts',(0.1301007483284,-1.,-2.07314114713047));
#30672=CARTESIAN_POINT('Ctrl Pts',(0.1301007483284,1.,-2.07314114713047));
#30673=CARTESIAN_POINT('Ctrl Pts',(0.127784445276116,-1.,-2.07892715110967));
#30674=CARTESIAN_POINT('Ctrl Pts',(0.127784445276116,1.,-2.07892715110967));
#30675=CARTESIAN_POINT('Ctrl Pts',(0.125423679412058,-1.,-2.08470840653628));
#30676=CARTESIAN_POINT('Ctrl Pts',(0.125423679412058,1.,-2.08470840653628));
#30677=CARTESIAN_POINT('Ctrl Pts',(0.123018905621083,-1.,-2.09048392424826));
#30678=CARTESIAN_POINT('Ctrl Pts',(0.123018905621083,1.,-2.09048392424826));
#30679=CARTESIAN_POINT('Ctrl Pts',(0.120570567965129,-1.,-2.09625292867756));
#30680=CARTESIAN_POINT('Ctrl Pts',(0.120570567965129,1.,-2.09625292867756));
#30681=CARTESIAN_POINT('Ctrl Pts',(0.118079107988368,-1.,-2.10201512132945));
#30682=CARTESIAN_POINT('Ctrl Pts',(0.118079107988368,1.,-2.10201512132945));
#30683=CARTESIAN_POINT('Ctrl Pts',(0.11554495768794,-1.,-2.10777050261359));
#30684=CARTESIAN_POINT('Ctrl Pts',(0.11554495768794,1.,-2.10777050261359));
#30685=CARTESIAN_POINT('Ctrl Pts',(0.112968534419746,-1.,-2.11351924490335));
#30686=CARTESIAN_POINT('Ctrl Pts',(0.112968534419746,1.,-2.11351924490335));
#30687=CARTESIAN_POINT('Ctrl Pts',(0.11035023613502,-1.,-2.11926155590849));
#30688=CARTESIAN_POINT('Ctrl Pts',(0.11035023613502,1.,-2.11926155590849));
#30689=CARTESIAN_POINT('Ctrl Pts',(0.107690435231068,-1.,-2.12499752306927));
#30690=CARTESIAN_POINT('Ctrl Pts',(0.107690435231068,1.,-2.12499752306927));
#30691=CARTESIAN_POINT('Ctrl Pts',(0.104989479152703,-1.,-2.1307270488718));
#30692=CARTESIAN_POINT('Ctrl Pts',(0.104989479152703,1.,-2.1307270488718));
#30693=CARTESIAN_POINT('Ctrl Pts',(0.102247700556064,-1.,-2.13644992667052));
#30694=CARTESIAN_POINT('Ctrl Pts',(0.102247700556064,1.,-2.13644992667052));
#30695=CARTESIAN_POINT('Ctrl Pts',(0.0994654261990743,-1.,-2.14216588395974));
#30696=CARTESIAN_POINT('Ctrl Pts',(0.0994654261990743,1.,-2.14216588395974));
#30697=CARTESIAN_POINT('Ctrl Pts',(0.0966429852305689,-1.,-2.14787463531864));
#30698=CARTESIAN_POINT('Ctrl Pts',(0.0966429852305689,1.,-2.14787463531864));
#30699=CARTESIAN_POINT('Ctrl Pts',(0.0937807218868345,-1.,-2.15357593978377));
#30700=CARTESIAN_POINT('Ctrl Pts',(0.0937807218868345,1.,-2.15357593978377));
#30701=CARTESIAN_POINT('Ctrl Pts',(0.0908789888108266,-1.,-2.15926961544808));
#30702=CARTESIAN_POINT('Ctrl Pts',(0.0908789888108266,1.,-2.15926961544808));
#30703=CARTESIAN_POINT('Ctrl Pts',(0.0879381291387823,-1.,-2.16495552645275));
#30704=CARTESIAN_POINT('Ctrl Pts',(0.0879381291387823,1.,-2.16495552645275));
#30705=CARTESIAN_POINT('Ctrl Pts',(0.0849584620835643,-1.,-2.17063357871031));
#30706=CARTESIAN_POINT('Ctrl Pts',(0.0849584620835643,1.,-2.17063357871031));
#30707=CARTESIAN_POINT('Ctrl Pts',(0.0819402680871939,-1.,-2.1763037121106));
#30708=CARTESIAN_POINT('Ctrl Pts',(0.0819402680871939,1.,-2.1763037121106));
#30709=CARTESIAN_POINT('Ctrl Pts',(0.0788837727683228,-1.,-2.18196589448304));
#30710=CARTESIAN_POINT('Ctrl Pts',(0.0788837727683228,1.,-2.18196589448304));
#30711=CARTESIAN_POINT('Ctrl Pts',(0.0757891465833411,-1.,-2.1876201139874));
#30712=CARTESIAN_POINT('Ctrl Pts',(0.0757891465833411,1.,-2.1876201139874));
#30713=CARTESIAN_POINT('Ctrl Pts',(0.0732830357304276,-1.,-2.19213712012956));
#30714=CARTESIAN_POINT('Ctrl Pts',(0.0732830357304276,1.,-2.19213712012956));
#30715=CARTESIAN_POINT('Ctrl Pts',(0.0713863779524627,-1.,-2.19552129483562));
#30716=CARTESIAN_POINT('Ctrl Pts',(0.0713863779524627,1.,-2.19552129483562));
#30717=CARTESIAN_POINT('Ctrl Pts',(0.0701143536324926,-1.,-2.19777582085261));
#30718=CARTESIAN_POINT('Ctrl Pts',(0.0701143536324926,1.,-2.19777582085261));
#30719=CARTESIAN_POINT('Ctrl Pts',(0.0694764450219584,-1.,-2.19890268624765));
#30720=CARTESIAN_POINT('Ctrl Pts',(0.0694764450219584,1.,-2.19890268624765));
#30721=CARTESIAN_POINT('',(0.163289472382896,1.,-1.74236521665491));
#30722=CARTESIAN_POINT('Ctrl Pts',(0.163289472382896,1.,-1.74236521665491));
#30723=CARTESIAN_POINT('Ctrl Pts',(0.163814161002474,1.,-1.74720349503904));
#30724=CARTESIAN_POINT('Ctrl Pts',(0.164834765708484,1.,-1.75666056640041));
#30725=CARTESIAN_POINT('Ctrl Pts',(0.166279355148738,1.,-1.77018771687692));
#30726=CARTESIAN_POINT('Ctrl Pts',(0.16803277280837,1.,-1.78690649988931));
#30727=CARTESIAN_POINT('Ctrl Pts',(0.169936923908078,1.,-1.80561530633924));
#30728=CARTESIAN_POINT('Ctrl Pts',(0.171554770207306,1.,-1.82215766815414));
#30729=CARTESIAN_POINT('Ctrl Pts',(0.17288944289442,1.,-1.83658380530747));
#30730=CARTESIAN_POINT('Ctrl Pts',(0.173946627589401,1.,-1.84898113200543));
#30731=CARTESIAN_POINT('Ctrl Pts',(0.174735259276856,1.,-1.85948367089838));
#30732=CARTESIAN_POINT('Ctrl Pts',(0.175268337590901,1.,-1.86828349694972));
#30733=CARTESIAN_POINT('Ctrl Pts',(0.175563480746205,1.,-1.87563767773249));
#30734=CARTESIAN_POINT('Ctrl Pts',(0.175644148889271,1.,-1.88188663144846));
#30735=CARTESIAN_POINT('Ctrl Pts',(0.175538155840286,1.,-1.88742606272818));
#30736=CARTESIAN_POINT('Ctrl Pts',(0.175274276190664,1.,-1.89264630198279));
#30737=CARTESIAN_POINT('Ctrl Pts',(0.174879405091277,1.,-1.89788101117148));
#30738=CARTESIAN_POINT('Ctrl Pts',(0.174375518661222,1.,-1.90335253863003));
#30739=CARTESIAN_POINT('Ctrl Pts',(0.173776635257984,1.,-1.90911693975475));
#30740=CARTESIAN_POINT('Ctrl Pts',(0.173090695383619,1.,-1.91511429159681));
#30741=CARTESIAN_POINT('Ctrl Pts',(0.172321621259557,1.,-1.92122334398034));
#30742=CARTESIAN_POINT('Ctrl Pts',(0.17147119153296,1.,-1.92731093582));
#30743=CARTESIAN_POINT('Ctrl Pts',(0.170541253116136,1.,-1.93329183155455));
#30744=CARTESIAN_POINT('Ctrl Pts',(0.169534904817425,1.,-1.93915639211497));
#30745=CARTESIAN_POINT('Ctrl Pts',(0.168455741607516,1.,-1.94493757756879));
#30746=CARTESIAN_POINT('Ctrl Pts',(0.167307501784469,1.,-1.95069027794286));
#30747=CARTESIAN_POINT('Ctrl Pts',(0.166093592002833,1.,-1.95646759718755));
#30748=CARTESIAN_POINT('Ctrl Pts',(0.1648165689203,1.,-1.96229379940174));
#30749=CARTESIAN_POINT('Ctrl Pts',(0.16347818545776,1.,-1.96816512678));
#30750=CARTESIAN_POINT('Ctrl Pts',(0.162079693556302,1.,-1.97406280235204));
#30751=CARTESIAN_POINT('Ctrl Pts',(0.16062206078461,1.,-1.97996195437557));
#30752=CARTESIAN_POINT('Ctrl Pts',(0.159106226437288,1.,-1.98584238283279));
#30753=CARTESIAN_POINT('Ctrl Pts',(0.157533331459215,1.,-1.99169810931893));
#30754=CARTESIAN_POINT('Ctrl Pts',(0.155904629548774,1.,-1.99753284771487));
#30755=CARTESIAN_POINT('Ctrl Pts',(0.154221403049719,1.,-2.00335565310539));
#30756=CARTESIAN_POINT('Ctrl Pts',(0.152484883621452,1.,-2.00917680318426));
#30757=CARTESIAN_POINT('Ctrl Pts',(0.150696157673084,1.,-2.01500291940243));
#30758=CARTESIAN_POINT('Ctrl Pts',(0.148856124775343,1.,-2.02083464969897));
#30759=CARTESIAN_POINT('Ctrl Pts',(0.146965557332586,1.,-2.02666926182017));
#30760=CARTESIAN_POINT('Ctrl Pts',(0.145025140186058,1.,-2.03250223739941));
#30761=CARTESIAN_POINT('Ctrl Pts',(0.143035515058208,1.,-2.03832911025913));
#30762=CARTESIAN_POINT('Ctrl Pts',(0.140997332152545,1.,-2.04414757947919));
#30763=CARTESIAN_POINT('Ctrl Pts',(0.138911255368966,1.,-2.04995762001333));
#30764=CARTESIAN_POINT('Ctrl Pts',(0.136777941218044,1.,-2.0557604441427));
#30765=CARTESIAN_POINT('Ctrl Pts',(0.134598026192107,1.,-2.06155781517844));
#30766=CARTESIAN_POINT('Ctrl Pts',(0.13237211154771,1.,-2.06735123910319));
#30767=CARTESIAN_POINT('Ctrl Pts',(0.1301007483284,1.,-2.07314114713047));
#30768=CARTESIAN_POINT('Ctrl Pts',(0.127784445276116,1.,-2.07892715110967));
#30769=CARTESIAN_POINT('Ctrl Pts',(0.125423679412058,1.,-2.08470840653628));
#30770=CARTESIAN_POINT('Ctrl Pts',(0.123018905621083,1.,-2.09048392424826));
#30771=CARTESIAN_POINT('Ctrl Pts',(0.120570567965129,1.,-2.09625292867756));
#30772=CARTESIAN_POINT('Ctrl Pts',(0.118079107988368,1.,-2.10201512132945));
#30773=CARTESIAN_POINT('Ctrl Pts',(0.11554495768794,1.,-2.10777050261359));
#30774=CARTESIAN_POINT('Ctrl Pts',(0.112968534419746,1.,-2.11351924490335));
#30775=CARTESIAN_POINT('Ctrl Pts',(0.11035023613502,1.,-2.11926155590849));
#30776=CARTESIAN_POINT('Ctrl Pts',(0.107690435231068,1.,-2.12499752306927));
#30777=CARTESIAN_POINT('Ctrl Pts',(0.104989479152703,1.,-2.1307270488718));
#30778=CARTESIAN_POINT('Ctrl Pts',(0.102247700556064,1.,-2.13644992667052));
#30779=CARTESIAN_POINT('Ctrl Pts',(0.0994654261990743,1.,-2.14216588395974));
#30780=CARTESIAN_POINT('Ctrl Pts',(0.0966429852305689,1.,-2.14787463531864));
#30781=CARTESIAN_POINT('Ctrl Pts',(0.0937807218868345,1.,-2.15357593978377));
#30782=CARTESIAN_POINT('Ctrl Pts',(0.0908789888108266,1.,-2.15926961544808));
#30783=CARTESIAN_POINT('Ctrl Pts',(0.0879381291387823,1.,-2.16495552645275));
#30784=CARTESIAN_POINT('Ctrl Pts',(0.0849584620835643,1.,-2.17063357871031));
#30785=CARTESIAN_POINT('Ctrl Pts',(0.0819402680871939,1.,-2.1763037121106));
#30786=CARTESIAN_POINT('Ctrl Pts',(0.0788837727683228,1.,-2.18196589448304));
#30787=CARTESIAN_POINT('Ctrl Pts',(0.0757891465833411,1.,-2.1876201139874));
#30788=CARTESIAN_POINT('Ctrl Pts',(0.0732830357304276,1.,-2.19213712012956));
#30789=CARTESIAN_POINT('Ctrl Pts',(0.0713863779524627,1.,-2.19552129483562));
#30790=CARTESIAN_POINT('Ctrl Pts',(0.0701143536324926,1.,-2.19777582085261));
#30791=CARTESIAN_POINT('Ctrl Pts',(0.0694764450219584,1.,-2.19890268624765));
#30792=CARTESIAN_POINT('',(0.163289472382896,0.,-1.74236521665491));
#30793=CARTESIAN_POINT('Origin',(0.,0.,0.));
#30794=CARTESIAN_POINT('',(0.383122945602004,1.,-1.7075470150345));
#30795=CARTESIAN_POINT('Origin',(0.,1.,0.));
#30796=CARTESIAN_POINT('',(0.383122945602004,0.,-1.7075470150345));
#30797=CARTESIAN_POINT('Ctrl Pts',(0.61342227326009,-1.,-2.11275013067528));
#30798=CARTESIAN_POINT('Ctrl Pts',(0.61342227326009,1.,-2.11275013067528));
#30799=CARTESIAN_POINT('Ctrl Pts',(0.61246736556225,-1.,-2.11187554260142));
#30800=CARTESIAN_POINT('Ctrl Pts',(0.61246736556225,1.,-2.11187554260142));
#30801=CARTESIAN_POINT('Ctrl Pts',(0.610560911691113,-1.,-2.11012443807661));
#30802=CARTESIAN_POINT('Ctrl Pts',(0.610560911691113,1.,-2.11012443807661));
#30803=CARTESIAN_POINT('Ctrl Pts',(0.607711315456826,-1.,-2.10749199615859));
#30804=CARTESIAN_POINT('Ctrl Pts',(0.607711315456826,1.,-2.10749199615859));
#30805=CARTESIAN_POINT('Ctrl Pts',(0.603932030738212,-1.,-2.10397049887709));
#30806=CARTESIAN_POINT('Ctrl Pts',(0.603932030738212,1.,-2.10397049887709));
#30807=CARTESIAN_POINT('Ctrl Pts',(0.599241616422144,-1.,-2.09954930865331));
#30808=CARTESIAN_POINT('Ctrl Pts',(0.599241616422144,1.,-2.09954930865331));
#30809=CARTESIAN_POINT('Ctrl Pts',(0.594585006052823,-1.,-2.09510876220501));
#30810=CARTESIAN_POINT('Ctrl Pts',(0.594585006052823,1.,-2.09510876220501));
#30811=CARTESIAN_POINT('Ctrl Pts',(0.589962365403189,-1.,-2.09064881812053));
#30812=CARTESIAN_POINT('Ctrl Pts',(0.589962365403189,1.,-2.09064881812053));
#30813=CARTESIAN_POINT('Ctrl Pts',(0.585373918990895,-1.,-2.086169437277));
#30814=CARTESIAN_POINT('Ctrl Pts',(0.585373918990895,1.,-2.086169437277));
#30815=CARTESIAN_POINT('Ctrl Pts',(0.580819952107256,-1.,-2.08167059018138));
#30816=CARTESIAN_POINT('Ctrl Pts',(0.580819952107256,1.,-2.08167059018138));
#30817=CARTESIAN_POINT('Ctrl Pts',(0.576300797416274,-1.,-2.07715226767361));
#30818=CARTESIAN_POINT('Ctrl Pts',(0.576300797416274,1.,-2.07715226767361));
#30819=CARTESIAN_POINT('Ctrl Pts',(0.571816823242411,-1.,-2.07261449292758));
#30820=CARTESIAN_POINT('Ctrl Pts',(0.571816823242411,1.,-2.07261449292758));
#30821=CARTESIAN_POINT('Ctrl Pts',(0.567368421181229,-1.,-2.06805732997383));
#30822=CARTESIAN_POINT('Ctrl Pts',(0.567368421181229,1.,-2.06805732997383));
#30823=CARTESIAN_POINT('Ctrl Pts',(0.562955993082574,-1.,-2.06348090160697));
#30824=CARTESIAN_POINT('Ctrl Pts',(0.562955993082574,1.,-2.06348090160697));
#30825=CARTESIAN_POINT('Ctrl Pts',(0.558579940185467,-1.,-2.05888537756571));
#30826=CARTESIAN_POINT('Ctrl Pts',(0.558579940185467,1.,-2.05888537756571));
#30827=CARTESIAN_POINT('Ctrl Pts',(0.554240657464109,-1.,-2.05427091604482));
#30828=CARTESIAN_POINT('Ctrl Pts',(0.554240657464109,1.,-2.05427091604482));
#30829=CARTESIAN_POINT('Ctrl Pts',(0.549938525150342,-1.,-2.04963761077974));
#30830=CARTESIAN_POINT('Ctrl Pts',(0.549938525150342,1.,-2.04963761077974));
#30831=CARTESIAN_POINT('Ctrl Pts',(0.545673903817348,-1.,-2.0449854471456));
#30832=CARTESIAN_POINT('Ctrl Pts',(0.545673903817348,1.,-2.0449854471456));
#30833=CARTESIAN_POINT('Ctrl Pts',(0.54144712061552,-1.,-2.0403142269048));
#30834=CARTESIAN_POINT('Ctrl Pts',(0.54144712061552,1.,-2.0403142269048));
#30835=CARTESIAN_POINT('Ctrl Pts',(0.537258489833134,-1.,-2.03562362953993));
#30836=CARTESIAN_POINT('Ctrl Pts',(0.537258489833134,1.,-2.03562362953993));
#30837=CARTESIAN_POINT('Ctrl Pts',(0.533108355132905,-1.,-2.03091336214401));
#30838=CARTESIAN_POINT('Ctrl Pts',(0.533108355132905,1.,-2.03091336214401));
#30839=CARTESIAN_POINT('Ctrl Pts',(0.52899712724191,-1.,-2.02618329083289));
#30840=CARTESIAN_POINT('Ctrl Pts',(0.52899712724191,1.,-2.02618329083289));
#30841=CARTESIAN_POINT('Ctrl Pts',(0.524925318333518,-1.,-2.02143356304712));
#30842=CARTESIAN_POINT('Ctrl Pts',(0.524925318333518,1.,-2.02143356304712));
#30843=CARTESIAN_POINT('Ctrl Pts',(0.520893590399428,-1.,-2.01666477917306));
#30844=CARTESIAN_POINT('Ctrl Pts',(0.520893590399428,1.,-2.01666477917306));
#30845=CARTESIAN_POINT('Ctrl Pts',(0.516902681728733,-1.,-2.01187773939257));
#30846=CARTESIAN_POINT('Ctrl Pts',(0.516902681728733,1.,-2.01187773939257));
#30847=CARTESIAN_POINT('Ctrl Pts',(0.512953306961813,-1.,-2.00707309946955));
#30848=CARTESIAN_POINT('Ctrl Pts',(0.512953306961813,1.,-2.00707309946955));
#30849=CARTESIAN_POINT('Ctrl Pts',(0.509046069886152,-1.,-2.00225107134733));
#30850=CARTESIAN_POINT('Ctrl Pts',(0.509046069886152,1.,-2.00225107134733));
#30851=CARTESIAN_POINT('Ctrl Pts',(0.505181361323011,-1.,-1.99741107463567));
#30852=CARTESIAN_POINT('Ctrl Pts',(0.505181361323011,1.,-1.99741107463567));
#30853=CARTESIAN_POINT('Ctrl Pts',(0.501359287727129,-1.,-1.9925514912615));
#30854=CARTESIAN_POINT('Ctrl Pts',(0.501359287727129,1.,-1.9925514912615));
#30855=CARTESIAN_POINT('Ctrl Pts',(0.497579909545564,-1.,-1.98767044752929));
#30856=CARTESIAN_POINT('Ctrl Pts',(0.497579909545564,1.,-1.98767044752929));
#30857=CARTESIAN_POINT('Ctrl Pts',(0.493843476541492,-1.,-1.9827665876182));
#30858=CARTESIAN_POINT('Ctrl Pts',(0.493843476541492,1.,-1.9827665876182));
#30859=CARTESIAN_POINT('Ctrl Pts',(0.490150627860955,-1.,-1.97783973019229));
#30860=CARTESIAN_POINT('Ctrl Pts',(0.490150627860955,1.,-1.97783973019229));
#30861=CARTESIAN_POINT('Ctrl Pts',(0.486502692907661,-1.,-1.97289186263272));
#30862=CARTESIAN_POINT('Ctrl Pts',(0.486502692907661,1.,-1.97289186263272));
#30863=CARTESIAN_POINT('Ctrl Pts',(0.482901662120686,-1.,-1.96792703422358));
#30864=CARTESIAN_POINT('Ctrl Pts',(0.482901662120686,1.,-1.96792703422358));
#30865=CARTESIAN_POINT('Ctrl Pts',(0.479349583074846,-1.,-1.96294933055938));
#30866=CARTESIAN_POINT('Ctrl Pts',(0.479349583074846,1.,-1.96294933055938));
#30867=CARTESIAN_POINT('Ctrl Pts',(0.475848034683171,-1.,-1.95796111148175));
#30868=CARTESIAN_POINT('Ctrl Pts',(0.475848034683171,1.,-1.95796111148175));
#30869=CARTESIAN_POINT('Ctrl Pts',(0.472397672264079,-1.,-1.95296148278136));
#30870=CARTESIAN_POINT('Ctrl Pts',(0.472397672264079,1.,-1.95296148278136));
#30871=CARTESIAN_POINT('Ctrl Pts',(0.468997482913158,-1.,-1.94794381136524));
#30872=CARTESIAN_POINT('Ctrl Pts',(0.468997482913158,1.,-1.94794381136524));
#30873=CARTESIAN_POINT('Ctrl Pts',(0.465645462026064,-1.,-1.94289794196205));
#30874=CARTESIAN_POINT('Ctrl Pts',(0.465645462026064,1.,-1.94289794196205));
#30875=CARTESIAN_POINT('Ctrl Pts',(0.462340031009087,-1.,-1.93781486640834));
#30876=CARTESIAN_POINT('Ctrl Pts',(0.462340031009087,1.,-1.93781486640834));
#30877=CARTESIAN_POINT('Ctrl Pts',(0.459081234547931,-1.,-1.93269066517936));
#30878=CARTESIAN_POINT('Ctrl Pts',(0.459081234547931,1.,-1.93269066517936));
#30879=CARTESIAN_POINT('Ctrl Pts',(0.455872005174335,-1.,-1.92753067150461));
#30880=CARTESIAN_POINT('Ctrl Pts',(0.455872005174335,1.,-1.92753067150461));
#30881=CARTESIAN_POINT('Ctrl Pts',(0.452719478359356,-1.,-1.9223538064847));
#30882=CARTESIAN_POINT('Ctrl Pts',(0.452719478359356,1.,-1.9223538064847));
#30883=CARTESIAN_POINT('Ctrl Pts',(0.449632260106572,-1.,-1.91718342555717));
#30884=CARTESIAN_POINT('Ctrl Pts',(0.449632260106572,1.,-1.91718342555717));
#30885=CARTESIAN_POINT('Ctrl Pts',(0.446617343485651,-1.,-1.91203699981095));
#30886=CARTESIAN_POINT('Ctrl Pts',(0.446617343485651,1.,-1.91203699981095));
#30887=CARTESIAN_POINT('Ctrl Pts',(0.44367755684917,-1.,-1.90691756144906));
#30888=CARTESIAN_POINT('Ctrl Pts',(0.44367755684917,1.,-1.90691756144906));
#30889=CARTESIAN_POINT('Ctrl Pts',(0.44080783370416,-1.,-1.90180124389137));
#30890=CARTESIAN_POINT('Ctrl Pts',(0.44080783370416,1.,-1.90180124389137));
#30891=CARTESIAN_POINT('Ctrl Pts',(0.437995003948443,-1.,-1.89663648956549));
#30892=CARTESIAN_POINT('Ctrl Pts',(0.437995003948443,1.,-1.89663648956549));
#30893=CARTESIAN_POINT('Ctrl Pts',(0.43522566096358,-1.,-1.89136993975585));
#30894=CARTESIAN_POINT('Ctrl Pts',(0.43522566096358,1.,-1.89136993975585));
#30895=CARTESIAN_POINT('Ctrl Pts',(0.432493038548833,-1.,-1.88596913666828));
#30896=CARTESIAN_POINT('Ctrl Pts',(0.432493038548833,1.,-1.88596913666828));
#30897=CARTESIAN_POINT('Ctrl Pts',(0.429803062482217,-1.,-1.88044229001779));
#30898=CARTESIAN_POINT('Ctrl Pts',(0.429803062482217,1.,-1.88044229001779));
#30899=CARTESIAN_POINT('Ctrl Pts',(0.427183828518743,-1.,-1.87486989291334));
#30900=CARTESIAN_POINT('Ctrl Pts',(0.427183828518743,1.,-1.87486989291334));
#30901=CARTESIAN_POINT('Ctrl Pts',(0.424678177290876,-1.,-1.8693780394412));
#30902=CARTESIAN_POINT('Ctrl Pts',(0.424678177290876,1.,-1.8693780394412));
#30903=CARTESIAN_POINT('Ctrl Pts',(0.422327307417884,-1.,-1.86408083333863));
#30904=CARTESIAN_POINT('Ctrl Pts',(0.422327307417884,1.,-1.86408083333863));
#30905=CARTESIAN_POINT('Ctrl Pts',(0.420157287975583,-1.,-1.8590328109667));
#30906=CARTESIAN_POINT('Ctrl Pts',(0.420157287975583,1.,-1.8590328109667));
#30907=CARTESIAN_POINT('Ctrl Pts',(0.418164129144045,-1.,-1.8541763285645));
#30908=CARTESIAN_POINT('Ctrl Pts',(0.418164129144045,1.,-1.8541763285645));
#30909=CARTESIAN_POINT('Ctrl Pts',(0.416300022039885,-1.,-1.84929312930314));
#30910=CARTESIAN_POINT('Ctrl Pts',(0.416300022039885,1.,-1.84929312930314));
#30911=CARTESIAN_POINT('Ctrl Pts',(0.414487438255542,-1.,-1.84405757074218));
#30912=CARTESIAN_POINT('Ctrl Pts',(0.414487438255542,1.,-1.84405757074218));
#30913=CARTESIAN_POINT('Ctrl Pts',(0.412633125322945,-1.,-1.8380895347617));
#30914=CARTESIAN_POINT('Ctrl Pts',(0.412633125322945,1.,-1.8380895347617));
#30915=CARTESIAN_POINT('Ctrl Pts',(0.410641256301276,-1.,-1.83100408895047));
#30916=CARTESIAN_POINT('Ctrl Pts',(0.410641256301276,1.,-1.83100408895047));
#30917=CARTESIAN_POINT('Ctrl Pts',(0.408428948106227,-1.,-1.82247022677562));
#30918=CARTESIAN_POINT('Ctrl Pts',(0.408428948106227,1.,-1.82247022677562));
#30919=CARTESIAN_POINT('Ctrl Pts',(0.405933518407175,-1.,-1.81223801812013));
#30920=CARTESIAN_POINT('Ctrl Pts',(0.405933518407175,1.,-1.81223801812013));
#30921=CARTESIAN_POINT('Ctrl Pts',(0.403107976163396,-1.,-1.80012077173238));
#30922=CARTESIAN_POINT('Ctrl Pts',(0.403107976163396,1.,-1.80012077173238));
#30923=CARTESIAN_POINT('Ctrl Pts',(0.399919403774155,-1.,-1.78598826343754));
#30924=CARTESIAN_POINT('Ctrl Pts',(0.399919403774155,1.,-1.78598826343754));
#30925=CARTESIAN_POINT('Ctrl Pts',(0.396346196110688,-1.,-1.76975560043442));
#30926=CARTESIAN_POINT('Ctrl Pts',(0.396346196110688,1.,-1.76975560043442));
#30927=CARTESIAN_POINT('Ctrl Pts',(0.392375812285395,-1.,-1.75137405310193));
#30928=CARTESIAN_POINT('Ctrl Pts',(0.392375812285395,1.,-1.75137405310193));
#30929=CARTESIAN_POINT('Ctrl Pts',(0.388877023502615,-1.,-1.73493170972829));
#30930=CARTESIAN_POINT('Ctrl Pts',(0.388877023502615,1.,-1.73493170972829));
#30931=CARTESIAN_POINT('Ctrl Pts',(0.386070790323281,-1.,-1.72162022244582));
#30932=CARTESIAN_POINT('Ctrl Pts',(0.386070790323281,1.,-1.72162022244582));
#30933=CARTESIAN_POINT('Ctrl Pts',(0.384119047314215,-1.,-1.71231062891398));
#30934=CARTESIAN_POINT('Ctrl Pts',(0.384119047314215,1.,-1.71231062891398));
#30935=CARTESIAN_POINT('Ctrl Pts',(0.383122945602004,-1.,-1.7075470150345));
#30936=CARTESIAN_POINT('Ctrl Pts',(0.383122945602004,1.,-1.7075470150345));
#30937=CARTESIAN_POINT('',(0.61342227326009,1.,-2.11275013067528));
#30938=CARTESIAN_POINT('Ctrl Pts',(0.61342227326009,1.,-2.11275013067528));
#30939=CARTESIAN_POINT('Ctrl Pts',(0.61246736556225,1.,-2.11187554260142));
#30940=CARTESIAN_POINT('Ctrl Pts',(0.610560911691113,1.,-2.11012443807661));
#30941=CARTESIAN_POINT('Ctrl Pts',(0.607711315456826,1.,-2.10749199615859));
#30942=CARTESIAN_POINT('Ctrl Pts',(0.603932030738212,1.,-2.10397049887709));
#30943=CARTESIAN_POINT('Ctrl Pts',(0.599241616422144,1.,-2.09954930865331));
#30944=CARTESIAN_POINT('Ctrl Pts',(0.594585006052823,1.,-2.09510876220501));
#30945=CARTESIAN_POINT('Ctrl Pts',(0.589962365403189,1.,-2.09064881812053));
#30946=CARTESIAN_POINT('Ctrl Pts',(0.585373918990895,1.,-2.086169437277));
#30947=CARTESIAN_POINT('Ctrl Pts',(0.580819952107256,1.,-2.08167059018138));
#30948=CARTESIAN_POINT('Ctrl Pts',(0.576300797416274,1.,-2.07715226767361));
#30949=CARTESIAN_POINT('Ctrl Pts',(0.571816823242411,1.,-2.07261449292758));
#30950=CARTESIAN_POINT('Ctrl Pts',(0.567368421181229,1.,-2.06805732997383));
#30951=CARTESIAN_POINT('Ctrl Pts',(0.562955993082574,1.,-2.06348090160697));
#30952=CARTESIAN_POINT('Ctrl Pts',(0.558579940185467,1.,-2.05888537756571));
#30953=CARTESIAN_POINT('Ctrl Pts',(0.554240657464109,1.,-2.05427091604482));
#30954=CARTESIAN_POINT('Ctrl Pts',(0.549938525150342,1.,-2.04963761077974));
#30955=CARTESIAN_POINT('Ctrl Pts',(0.545673903817348,1.,-2.0449854471456));
#30956=CARTESIAN_POINT('Ctrl Pts',(0.54144712061552,1.,-2.0403142269048));
#30957=CARTESIAN_POINT('Ctrl Pts',(0.537258489833134,1.,-2.03562362953993));
#30958=CARTESIAN_POINT('Ctrl Pts',(0.533108355132905,1.,-2.03091336214401));
#30959=CARTESIAN_POINT('Ctrl Pts',(0.52899712724191,1.,-2.02618329083289));
#30960=CARTESIAN_POINT('Ctrl Pts',(0.524925318333518,1.,-2.02143356304712));
#30961=CARTESIAN_POINT('Ctrl Pts',(0.520893590399428,1.,-2.01666477917306));
#30962=CARTESIAN_POINT('Ctrl Pts',(0.516902681728733,1.,-2.01187773939257));
#30963=CARTESIAN_POINT('Ctrl Pts',(0.512953306961813,1.,-2.00707309946955));
#30964=CARTESIAN_POINT('Ctrl Pts',(0.509046069886152,1.,-2.00225107134733));
#30965=CARTESIAN_POINT('Ctrl Pts',(0.505181361323011,1.,-1.99741107463567));
#30966=CARTESIAN_POINT('Ctrl Pts',(0.501359287727129,1.,-1.9925514912615));
#30967=CARTESIAN_POINT('Ctrl Pts',(0.497579909545564,1.,-1.98767044752929));
#30968=CARTESIAN_POINT('Ctrl Pts',(0.493843476541492,1.,-1.9827665876182));
#30969=CARTESIAN_POINT('Ctrl Pts',(0.490150627860955,1.,-1.97783973019229));
#30970=CARTESIAN_POINT('Ctrl Pts',(0.486502692907661,1.,-1.97289186263272));
#30971=CARTESIAN_POINT('Ctrl Pts',(0.482901662120686,1.,-1.96792703422358));
#30972=CARTESIAN_POINT('Ctrl Pts',(0.479349583074846,1.,-1.96294933055938));
#30973=CARTESIAN_POINT('Ctrl Pts',(0.475848034683171,1.,-1.95796111148175));
#30974=CARTESIAN_POINT('Ctrl Pts',(0.472397672264079,1.,-1.95296148278136));
#30975=CARTESIAN_POINT('Ctrl Pts',(0.468997482913158,1.,-1.94794381136524));
#30976=CARTESIAN_POINT('Ctrl Pts',(0.465645462026064,1.,-1.94289794196205));
#30977=CARTESIAN_POINT('Ctrl Pts',(0.462340031009087,1.,-1.93781486640834));
#30978=CARTESIAN_POINT('Ctrl Pts',(0.459081234547931,1.,-1.93269066517936));
#30979=CARTESIAN_POINT('Ctrl Pts',(0.455872005174335,1.,-1.92753067150461));
#30980=CARTESIAN_POINT('Ctrl Pts',(0.452719478359356,1.,-1.9223538064847));
#30981=CARTESIAN_POINT('Ctrl Pts',(0.449632260106572,1.,-1.91718342555717));
#30982=CARTESIAN_POINT('Ctrl Pts',(0.446617343485651,1.,-1.91203699981095));
#30983=CARTESIAN_POINT('Ctrl Pts',(0.44367755684917,1.,-1.90691756144906));
#30984=CARTESIAN_POINT('Ctrl Pts',(0.44080783370416,1.,-1.90180124389137));
#30985=CARTESIAN_POINT('Ctrl Pts',(0.437995003948443,1.,-1.89663648956549));
#30986=CARTESIAN_POINT('Ctrl Pts',(0.43522566096358,1.,-1.89136993975585));
#30987=CARTESIAN_POINT('Ctrl Pts',(0.432493038548833,1.,-1.88596913666828));
#30988=CARTESIAN_POINT('Ctrl Pts',(0.429803062482217,1.,-1.88044229001779));
#30989=CARTESIAN_POINT('Ctrl Pts',(0.427183828518743,1.,-1.87486989291334));
#30990=CARTESIAN_POINT('Ctrl Pts',(0.424678177290876,1.,-1.8693780394412));
#30991=CARTESIAN_POINT('Ctrl Pts',(0.422327307417884,1.,-1.86408083333863));
#30992=CARTESIAN_POINT('Ctrl Pts',(0.420157287975583,1.,-1.8590328109667));
#30993=CARTESIAN_POINT('Ctrl Pts',(0.418164129144045,1.,-1.8541763285645));
#30994=CARTESIAN_POINT('Ctrl Pts',(0.416300022039885,1.,-1.84929312930314));
#30995=CARTESIAN_POINT('Ctrl Pts',(0.414487438255542,1.,-1.84405757074218));
#30996=CARTESIAN_POINT('Ctrl Pts',(0.412633125322945,1.,-1.8380895347617));
#30997=CARTESIAN_POINT('Ctrl Pts',(0.410641256301276,1.,-1.83100408895047));
#30998=CARTESIAN_POINT('Ctrl Pts',(0.408428948106227,1.,-1.82247022677562));
#30999=CARTESIAN_POINT('Ctrl Pts',(0.405933518407175,1.,-1.81223801812013));
#31000=CARTESIAN_POINT('Ctrl Pts',(0.403107976163396,1.,-1.80012077173238));
#31001=CARTESIAN_POINT('Ctrl Pts',(0.399919403774155,1.,-1.78598826343754));
#31002=CARTESIAN_POINT('Ctrl Pts',(0.396346196110688,1.,-1.76975560043442));
#31003=CARTESIAN_POINT('Ctrl Pts',(0.392375812285395,1.,-1.75137405310193));
#31004=CARTESIAN_POINT('Ctrl Pts',(0.388877023502615,1.,-1.73493170972829));
#31005=CARTESIAN_POINT('Ctrl Pts',(0.386070790323281,1.,-1.72162022244582));
#31006=CARTESIAN_POINT('Ctrl Pts',(0.384119047314215,1.,-1.71231062891398));
#31007=CARTESIAN_POINT('Ctrl Pts',(0.383122945602004,1.,-1.7075470150345));
#31008=CARTESIAN_POINT('',(0.61342227326009,0.,-2.11275013067528));
#31009=CARTESIAN_POINT('Origin',(0.745574324794401,0.,-2.0698113262342));
#31010=CARTESIAN_POINT('',(0.745574324794401,1.,-2.0698113262342));
#31011=CARTESIAN_POINT('',(0.61342227326009,1.,-2.11275013067528));
#31012=CARTESIAN_POINT('',(0.745574324794401,0.,-2.0698113262342));
#31013=CARTESIAN_POINT('Ctrl Pts',(0.693717979106306,-1.,-1.60662857109684));
#31014=CARTESIAN_POINT('Ctrl Pts',(0.693717979106306,1.,-1.60662857109684));
#31015=CARTESIAN_POINT('Ctrl Pts',(0.695712097881194,-1.,-1.61106790958151));
#31016=CARTESIAN_POINT('Ctrl Pts',(0.695712097881194,1.,-1.61106790958151));
#31017=CARTESIAN_POINT('Ctrl Pts',(0.699605146405088,-1.,-1.61974673472612));
#31018=CARTESIAN_POINT('Ctrl Pts',(0.699605146405088,1.,-1.61974673472612));
#31019=CARTESIAN_POINT('Ctrl Pts',(0.705159151988319,-1.,-1.63216541664676));
#31020=CARTESIAN_POINT('Ctrl Pts',(0.705159151988319,1.,-1.63216541664676));
#31021=CARTESIAN_POINT('Ctrl Pts',(0.711993139355394,-1.,-1.64752408832016));
#31022=CARTESIAN_POINT('Ctrl Pts',(0.711993139355394,1.,-1.64752408832016));
#31023=CARTESIAN_POINT('Ctrl Pts',(0.719585433804282,-1.,-1.6647288055568));
#31024=CARTESIAN_POINT('Ctrl Pts',(0.719585433804282,1.,-1.6647288055568));
#31025=CARTESIAN_POINT('Ctrl Pts',(0.726235967997433,-1.,-1.67996158455503));
#31026=CARTESIAN_POINT('Ctrl Pts',(0.726235967997433,1.,-1.67996158455503));
#31027=CARTESIAN_POINT('Ctrl Pts',(0.731963238697195,-1.,-1.69326921975743));
#31028=CARTESIAN_POINT('Ctrl Pts',(0.731963238697195,1.,-1.69326921975743));
#31029=CARTESIAN_POINT('Ctrl Pts',(0.736799665724771,-1.,-1.70473309006121));
#31030=CARTESIAN_POINT('Ctrl Pts',(0.736799665724771,1.,-1.70473309006121));
#31031=CARTESIAN_POINT('Ctrl Pts',(0.740795162032087,-1.,-1.71447789751927));
#31032=CARTESIAN_POINT('Ctrl Pts',(0.740795162032087,1.,-1.71447789751927));
#31033=CARTESIAN_POINT('Ctrl Pts',(0.744021445433764,-1.,-1.7226822991693));
#31034=CARTESIAN_POINT('Ctrl Pts',(0.744021445433764,1.,-1.7226822991693));
#31035=CARTESIAN_POINT('Ctrl Pts',(0.746574710096436,-1.,-1.72958533647399));
#31036=CARTESIAN_POINT('Ctrl Pts',(0.746574710096436,1.,-1.72958533647399));
#31037=CARTESIAN_POINT('Ctrl Pts',(0.748582462954854,-1.,-1.73550351679848));
#31038=CARTESIAN_POINT('Ctrl Pts',(0.748582462954854,1.,-1.73550351679848));
#31039=CARTESIAN_POINT('Ctrl Pts',(0.75019343597954,-1.,-1.74080458266705));
#31040=CARTESIAN_POINT('Ctrl Pts',(0.75019343597954,1.,-1.74080458266705));
#31041=CARTESIAN_POINT('Ctrl Pts',(0.751555614163629,-1.,-1.74585086852298));
#31042=CARTESIAN_POINT('Ctrl Pts',(0.751555614163629,1.,-1.74585086852298));
#31043=CARTESIAN_POINT('Ctrl Pts',(0.752797683531377,-1.,-1.75095139468809));
#31044=CARTESIAN_POINT('Ctrl Pts',(0.752797683531377,1.,-1.75095139468809));
#31045=CARTESIAN_POINT('Ctrl Pts',(0.75400925402848,-1.,-1.75631083600175));
#31046=CARTESIAN_POINT('Ctrl Pts',(0.75400925402848,1.,-1.75631083600175));
#31047=CARTESIAN_POINT('Ctrl Pts',(0.755220979975262,-1.,-1.7619781724032));
#31048=CARTESIAN_POINT('Ctrl Pts',(0.755220979975262,1.,-1.7619781724032));
#31049=CARTESIAN_POINT('Ctrl Pts',(0.756421896028403,-1.,-1.76789396003141));
#31050=CARTESIAN_POINT('Ctrl Pts',(0.756421896028403,1.,-1.76789396003141));
#31051=CARTESIAN_POINT('Ctrl Pts',(0.757578264077238,-1.,-1.77394167108342));
#31052=CARTESIAN_POINT('Ctrl Pts',(0.757578264077238,1.,-1.77394167108342));
#31053=CARTESIAN_POINT('Ctrl Pts',(0.75865062667738,-1.,-1.77999411220912));
#31054=CARTESIAN_POINT('Ctrl Pts',(0.75865062667738,1.,-1.77999411220912));
#31055=CARTESIAN_POINT('Ctrl Pts',(0.759614401109868,-1.,-1.78596964884527));
#31056=CARTESIAN_POINT('Ctrl Pts',(0.759614401109868,1.,-1.78596964884527));
#31057=CARTESIAN_POINT('Ctrl Pts',(0.760469555880425,-1.,-1.79185815610802));
#31058=CARTESIAN_POINT('Ctrl Pts',(0.760469555880425,1.,-1.79185815610802));
#31059=CARTESIAN_POINT('Ctrl Pts',(0.761229695230359,-1.,-1.79768986997735));
#31060=CARTESIAN_POINT('Ctrl Pts',(0.761229695230359,1.,-1.79768986997735));
#31061=CARTESIAN_POINT('Ctrl Pts',(0.761915336443515,-1.,-1.80351583877334));
#31062=CARTESIAN_POINT('Ctrl Pts',(0.761915336443515,1.,-1.80351583877334));
#31063=CARTESIAN_POINT('Ctrl Pts',(0.762546129464036,-1.,-1.80938551463989));
#31064=CARTESIAN_POINT('Ctrl Pts',(0.762546129464036,1.,-1.80938551463989));
#31065=CARTESIAN_POINT('Ctrl Pts',(0.763132003836783,-1.,-1.81532118405566));
#31066=CARTESIAN_POINT('Ctrl Pts',(0.763132003836783,1.,-1.81532118405566));
#31067=CARTESIAN_POINT('Ctrl Pts',(0.763673465462854,-1.,-1.82131873145297));
#31068=CARTESIAN_POINT('Ctrl Pts',(0.763673465462854,1.,-1.82131873145297));
#31069=CARTESIAN_POINT('Ctrl Pts',(0.764165902606055,-1.,-1.8273599120008));
#31070=CARTESIAN_POINT('Ctrl Pts',(0.764165902606055,1.,-1.8273599120008));
#31071=CARTESIAN_POINT('Ctrl Pts',(0.764602549687845,-1.,-1.8334207722714));
#31072=CARTESIAN_POINT('Ctrl Pts',(0.764602549687845,1.,-1.8334207722714));
#31073=CARTESIAN_POINT('Ctrl Pts',(0.764978057881687,-1.,-1.83948181064823));
#31074=CARTESIAN_POINT('Ctrl Pts',(0.764978057881687,1.,-1.83948181064823));
#31075=CARTESIAN_POINT('Ctrl Pts',(0.765291664861971,-1.,-1.84553698875911));
#31076=CARTESIAN_POINT('Ctrl Pts',(0.765291664861971,1.,-1.84553698875911));
#31077=CARTESIAN_POINT('Ctrl Pts',(0.765545710619023,-1.,-1.85158945130054));
#31078=CARTESIAN_POINT('Ctrl Pts',(0.765545710619023,1.,-1.85158945130054));
#31079=CARTESIAN_POINT('Ctrl Pts',(0.765744212909305,-1.,-1.85764741390391));
#31080=CARTESIAN_POINT('Ctrl Pts',(0.765744212909305,1.,-1.85764741390391));
#31081=CARTESIAN_POINT('Ctrl Pts',(0.765891519092557,-1.,-1.86372027063315));
#31082=CARTESIAN_POINT('Ctrl Pts',(0.765891519092557,1.,-1.86372027063315));
#31083=CARTESIAN_POINT('Ctrl Pts',(0.765990708546111,-1.,-1.86981398314345));
#31084=CARTESIAN_POINT('Ctrl Pts',(0.765990708546111,1.,-1.86981398314345));
#31085=CARTESIAN_POINT('Ctrl Pts',(0.766042837036759,-1.,-1.87592888967886));
#31086=CARTESIAN_POINT('Ctrl Pts',(0.766042837036759,1.,-1.87592888967886));
#31087=CARTESIAN_POINT('Ctrl Pts',(0.766047794851868,-1.,-1.88206215302561));
#31088=CARTESIAN_POINT('Ctrl Pts',(0.766047794851868,1.,-1.88206215302561));
#31089=CARTESIAN_POINT('Ctrl Pts',(0.76600483706209,-1.,-1.88820926433409));
#31090=CARTESIAN_POINT('Ctrl Pts',(0.76600483706209,1.,-1.88820926433409));
#31091=CARTESIAN_POINT('Ctrl Pts',(0.765913193856979,-1.,-1.89436577771389));
#31092=CARTESIAN_POINT('Ctrl Pts',(0.765913193856979,1.,-1.89436577771389));
#31093=CARTESIAN_POINT('Ctrl Pts',(0.765772772593395,-1.,-1.90052930393599));
#31094=CARTESIAN_POINT('Ctrl Pts',(0.765772772593395,1.,-1.90052930393599));
#31095=CARTESIAN_POINT('Ctrl Pts',(0.765584196937936,-1.,-1.90669961402362));
#31096=CARTESIAN_POINT('Ctrl Pts',(0.765584196937936,1.,-1.90669961402362));
#31097=CARTESIAN_POINT('Ctrl Pts',(0.765348465884739,-1.,-1.91287765805174));
#31098=CARTESIAN_POINT('Ctrl Pts',(0.765348465884739,1.,-1.91287765805174));
#31099=CARTESIAN_POINT('Ctrl Pts',(0.765066729667095,-1.,-1.91906491634197));
#31100=CARTESIAN_POINT('Ctrl Pts',(0.765066729667095,1.,-1.91906491634197));
#31101=CARTESIAN_POINT('Ctrl Pts',(0.764740025488189,-1.,-1.92526263537041));
#31102=CARTESIAN_POINT('Ctrl Pts',(0.764740025488189,1.,-1.92526263537041));
#31103=CARTESIAN_POINT('Ctrl Pts',(0.764369010673889,-1.,-1.93147105496367));
#31104=CARTESIAN_POINT('Ctrl Pts',(0.764369010673889,1.,-1.93147105496367));
#31105=CARTESIAN_POINT('Ctrl Pts',(0.763954049121393,-1.,-1.93768964875867));
#31106=CARTESIAN_POINT('Ctrl Pts',(0.763954049121393,1.,-1.93768964875867));
#31107=CARTESIAN_POINT('Ctrl Pts',(0.76349533353858,-1.,-1.94391746617626));
#31108=CARTESIAN_POINT('Ctrl Pts',(0.76349533353858,1.,-1.94391746617626));
#31109=CARTESIAN_POINT('Ctrl Pts',(0.762992990878774,-1.,-1.95015342590025));
#31110=CARTESIAN_POINT('Ctrl Pts',(0.762992990878774,1.,-1.95015342590025));
#31111=CARTESIAN_POINT('Ctrl Pts',(0.762447203806263,-1.,-1.95639665309893));
#31112=CARTESIAN_POINT('Ctrl Pts',(0.762447203806263,1.,-1.95639665309893));
#31113=CARTESIAN_POINT('Ctrl Pts',(0.761858300014575,-1.,-1.96264672744229));
#31114=CARTESIAN_POINT('Ctrl Pts',(0.761858300014575,1.,-1.96264672744229));
#31115=CARTESIAN_POINT('Ctrl Pts',(0.761226690483986,-1.,-1.96890351582545));
#31116=CARTESIAN_POINT('Ctrl Pts',(0.761226690483986,1.,-1.96890351582545));
#31117=CARTESIAN_POINT('Ctrl Pts',(0.760552825409855,-1.,-1.97516705321521));
#31118=CARTESIAN_POINT('Ctrl Pts',(0.760552825409855,1.,-1.97516705321521));
#31119=CARTESIAN_POINT('Ctrl Pts',(0.759837147452135,-1.,-1.98143741418156));
#31120=CARTESIAN_POINT('Ctrl Pts',(0.759837147452135,1.,-1.98143741418156));
#31121=CARTESIAN_POINT('Ctrl Pts',(0.759080037802242,-1.,-1.98771456680806));
#31122=CARTESIAN_POINT('Ctrl Pts',(0.759080037802242,1.,-1.98771456680806));
#31123=CARTESIAN_POINT('Ctrl Pts',(0.758281796766377,-1.,-1.9939983109871));
#31124=CARTESIAN_POINT('Ctrl Pts',(0.758281796766377,1.,-1.9939983109871));
#31125=CARTESIAN_POINT('Ctrl Pts',(0.757442676862341,-1.,-2.00028834739072));
#31126=CARTESIAN_POINT('Ctrl Pts',(0.757442676862341,1.,-2.00028834739072));
#31127=CARTESIAN_POINT('Ctrl Pts',(0.756562904646496,-1.,-2.00658431587682));
#31128=CARTESIAN_POINT('Ctrl Pts',(0.756562904646496,1.,-2.00658431587682));
#31129=CARTESIAN_POINT('Ctrl Pts',(0.7556427049581,-1.,-2.01288584328149));
#31130=CARTESIAN_POINT('Ctrl Pts',(0.7556427049581,1.,-2.01288584328149));
#31131=CARTESIAN_POINT('Ctrl Pts',(0.75468233072352,-1.,-2.01919259406003));
#31132=CARTESIAN_POINT('Ctrl Pts',(0.75468233072352,1.,-2.01919259406003));
#31133=CARTESIAN_POINT('Ctrl Pts',(0.753682061113765,-1.,-2.02550428623587));
#31134=CARTESIAN_POINT('Ctrl Pts',(0.753682061113765,1.,-2.02550428623587));
#31135=CARTESIAN_POINT('Ctrl Pts',(0.752642180488104,-1.,-2.03182068456467));
#31136=CARTESIAN_POINT('Ctrl Pts',(0.752642180488104,1.,-2.03182068456467));
#31137=CARTESIAN_POINT('Ctrl Pts',(0.751562963361383,-1.,-2.03814160092173));
#31138=CARTESIAN_POINT('Ctrl Pts',(0.751562963361383,1.,-2.03814160092173));
#31139=CARTESIAN_POINT('Ctrl Pts',(0.750444657874758,-1.,-2.04446689147754));
#31140=CARTESIAN_POINT('Ctrl Pts',(0.750444657874758,1.,-2.04446689147754));
#31141=CARTESIAN_POINT('Ctrl Pts',(0.749287468663053,-1.,-2.05079645591606));
#31142=CARTESIAN_POINT('Ctrl Pts',(0.749287468663053,1.,-2.05079645591606));
#31143=CARTESIAN_POINT('Ctrl Pts',(0.748091554181101,-1.,-2.05713023030263));
#31144=CARTESIAN_POINT('Ctrl Pts',(0.748091554181101,1.,-2.05713023030263));
#31145=CARTESIAN_POINT('Ctrl Pts',(0.747103932785504,-1.,-2.06220058927162));
#31146=CARTESIAN_POINT('Ctrl Pts',(0.747103932785504,1.,-2.06220058927162));
#31147=CARTESIAN_POINT('Ctrl Pts',(0.746345871542695,-1.,-2.06600523016401));
#31148=CARTESIAN_POINT('Ctrl Pts',(0.746345871542695,1.,-2.06600523016401));
#31149=CARTESIAN_POINT('Ctrl Pts',(0.74583279137781,-1.,-2.06854248895575));
#31150=CARTESIAN_POINT('Ctrl Pts',(0.74583279137781,1.,-2.06854248895575));
#31151=CARTESIAN_POINT('Ctrl Pts',(0.745574324794401,-1.,-2.0698113262342));
#31152=CARTESIAN_POINT('Ctrl Pts',(0.745574324794401,1.,-2.0698113262342));
#31153=CARTESIAN_POINT('',(0.693717979106306,1.,-1.60662857109684));
#31154=CARTESIAN_POINT('Ctrl Pts',(0.693717979106306,1.,-1.60662857109684));
#31155=CARTESIAN_POINT('Ctrl Pts',(0.695712097881194,1.,-1.61106790958151));
#31156=CARTESIAN_POINT('Ctrl Pts',(0.699605146405088,1.,-1.61974673472612));
#31157=CARTESIAN_POINT('Ctrl Pts',(0.705159151988319,1.,-1.63216541664676));
#31158=CARTESIAN_POINT('Ctrl Pts',(0.711993139355394,1.,-1.64752408832016));
#31159=CARTESIAN_POINT('Ctrl Pts',(0.719585433804282,1.,-1.6647288055568));
#31160=CARTESIAN_POINT('Ctrl Pts',(0.726235967997433,1.,-1.67996158455503));
#31161=CARTESIAN_POINT('Ctrl Pts',(0.731963238697195,1.,-1.69326921975743));
#31162=CARTESIAN_POINT('Ctrl Pts',(0.736799665724771,1.,-1.70473309006121));
#31163=CARTESIAN_POINT('Ctrl Pts',(0.740795162032087,1.,-1.71447789751927));
#31164=CARTESIAN_POINT('Ctrl Pts',(0.744021445433764,1.,-1.7226822991693));
#31165=CARTESIAN_POINT('Ctrl Pts',(0.746574710096436,1.,-1.72958533647399));
#31166=CARTESIAN_POINT('Ctrl Pts',(0.748582462954854,1.,-1.73550351679848));
#31167=CARTESIAN_POINT('Ctrl Pts',(0.75019343597954,1.,-1.74080458266705));
#31168=CARTESIAN_POINT('Ctrl Pts',(0.751555614163629,1.,-1.74585086852298));
#31169=CARTESIAN_POINT('Ctrl Pts',(0.752797683531377,1.,-1.75095139468809));
#31170=CARTESIAN_POINT('Ctrl Pts',(0.75400925402848,1.,-1.75631083600175));
#31171=CARTESIAN_POINT('Ctrl Pts',(0.755220979975262,1.,-1.7619781724032));
#31172=CARTESIAN_POINT('Ctrl Pts',(0.756421896028403,1.,-1.76789396003141));
#31173=CARTESIAN_POINT('Ctrl Pts',(0.757578264077238,1.,-1.77394167108342));
#31174=CARTESIAN_POINT('Ctrl Pts',(0.75865062667738,1.,-1.77999411220912));
#31175=CARTESIAN_POINT('Ctrl Pts',(0.759614401109868,1.,-1.78596964884527));
#31176=CARTESIAN_POINT('Ctrl Pts',(0.760469555880425,1.,-1.79185815610802));
#31177=CARTESIAN_POINT('Ctrl Pts',(0.761229695230359,1.,-1.79768986997735));
#31178=CARTESIAN_POINT('Ctrl Pts',(0.761915336443515,1.,-1.80351583877334));
#31179=CARTESIAN_POINT('Ctrl Pts',(0.762546129464036,1.,-1.80938551463989));
#31180=CARTESIAN_POINT('Ctrl Pts',(0.763132003836783,1.,-1.81532118405566));
#31181=CARTESIAN_POINT('Ctrl Pts',(0.763673465462854,1.,-1.82131873145297));
#31182=CARTESIAN_POINT('Ctrl Pts',(0.764165902606055,1.,-1.8273599120008));
#31183=CARTESIAN_POINT('Ctrl Pts',(0.764602549687845,1.,-1.8334207722714));
#31184=CARTESIAN_POINT('Ctrl Pts',(0.764978057881687,1.,-1.83948181064823));
#31185=CARTESIAN_POINT('Ctrl Pts',(0.765291664861971,1.,-1.84553698875911));
#31186=CARTESIAN_POINT('Ctrl Pts',(0.765545710619023,1.,-1.85158945130054));
#31187=CARTESIAN_POINT('Ctrl Pts',(0.765744212909305,1.,-1.85764741390391));
#31188=CARTESIAN_POINT('Ctrl Pts',(0.765891519092557,1.,-1.86372027063315));
#31189=CARTESIAN_POINT('Ctrl Pts',(0.765990708546111,1.,-1.86981398314345));
#31190=CARTESIAN_POINT('Ctrl Pts',(0.766042837036759,1.,-1.87592888967886));
#31191=CARTESIAN_POINT('Ctrl Pts',(0.766047794851868,1.,-1.88206215302561));
#31192=CARTESIAN_POINT('Ctrl Pts',(0.76600483706209,1.,-1.88820926433409));
#31193=CARTESIAN_POINT('Ctrl Pts',(0.765913193856979,1.,-1.89436577771389));
#31194=CARTESIAN_POINT('Ctrl Pts',(0.765772772593395,1.,-1.90052930393599));
#31195=CARTESIAN_POINT('Ctrl Pts',(0.765584196937936,1.,-1.90669961402362));
#31196=CARTESIAN_POINT('Ctrl Pts',(0.765348465884739,1.,-1.91287765805174));
#31197=CARTESIAN_POINT('Ctrl Pts',(0.765066729667095,1.,-1.91906491634197));
#31198=CARTESIAN_POINT('Ctrl Pts',(0.764740025488189,1.,-1.92526263537041));
#31199=CARTESIAN_POINT('Ctrl Pts',(0.764369010673889,1.,-1.93147105496367));
#31200=CARTESIAN_POINT('Ctrl Pts',(0.763954049121393,1.,-1.93768964875867));
#31201=CARTESIAN_POINT('Ctrl Pts',(0.76349533353858,1.,-1.94391746617626));
#31202=CARTESIAN_POINT('Ctrl Pts',(0.762992990878774,1.,-1.95015342590025));
#31203=CARTESIAN_POINT('Ctrl Pts',(0.762447203806263,1.,-1.95639665309893));
#31204=CARTESIAN_POINT('Ctrl Pts',(0.761858300014575,1.,-1.96264672744229));
#31205=CARTESIAN_POINT('Ctrl Pts',(0.761226690483986,1.,-1.96890351582545));
#31206=CARTESIAN_POINT('Ctrl Pts',(0.760552825409855,1.,-1.97516705321521));
#31207=CARTESIAN_POINT('Ctrl Pts',(0.759837147452135,1.,-1.98143741418156));
#31208=CARTESIAN_POINT('Ctrl Pts',(0.759080037802242,1.,-1.98771456680806));
#31209=CARTESIAN_POINT('Ctrl Pts',(0.758281796766377,1.,-1.9939983109871));
#31210=CARTESIAN_POINT('Ctrl Pts',(0.757442676862341,1.,-2.00028834739072));
#31211=CARTESIAN_POINT('Ctrl Pts',(0.756562904646496,1.,-2.00658431587682));
#31212=CARTESIAN_POINT('Ctrl Pts',(0.7556427049581,1.,-2.01288584328149));
#31213=CARTESIAN_POINT('Ctrl Pts',(0.75468233072352,1.,-2.01919259406003));
#31214=CARTESIAN_POINT('Ctrl Pts',(0.753682061113765,1.,-2.02550428623587));
#31215=CARTESIAN_POINT('Ctrl Pts',(0.752642180488104,1.,-2.03182068456467));
#31216=CARTESIAN_POINT('Ctrl Pts',(0.751562963361383,1.,-2.03814160092173));
#31217=CARTESIAN_POINT('Ctrl Pts',(0.750444657874758,1.,-2.04446689147754));
#31218=CARTESIAN_POINT('Ctrl Pts',(0.749287468663053,1.,-2.05079645591606));
#31219=CARTESIAN_POINT('Ctrl Pts',(0.748091554181101,1.,-2.05713023030263));
#31220=CARTESIAN_POINT('Ctrl Pts',(0.747103932785504,1.,-2.06220058927162));
#31221=CARTESIAN_POINT('Ctrl Pts',(0.746345871542695,1.,-2.06600523016401));
#31222=CARTESIAN_POINT('Ctrl Pts',(0.74583279137781,1.,-2.06854248895575));
#31223=CARTESIAN_POINT('Ctrl Pts',(0.745574324794401,1.,-2.0698113262342));
#31224=CARTESIAN_POINT('',(0.693717979106306,0.,-1.60662857109684));
#31225=CARTESIAN_POINT('Origin',(0.,0.,0.));
#31226=CARTESIAN_POINT('',(0.892032620296855,1.,-1.5055822144029));
#31227=CARTESIAN_POINT('Origin',(0.,1.,0.));
#31228=CARTESIAN_POINT('',(0.892032620296855,0.,-1.5055822144029));
#31229=CARTESIAN_POINT('Ctrl Pts',(1.23627494547115,-1.,-1.81978687191668));
#31230=CARTESIAN_POINT('Ctrl Pts',(1.23627494547115,1.,-1.81978687191668));
#31231=CARTESIAN_POINT('Ctrl Pts',(1.23509651170476,-1.,-1.81925017193666));
#31232=CARTESIAN_POINT('Ctrl Pts',(1.23509651170476,1.,-1.81925017193666));
#31233=CARTESIAN_POINT('Ctrl Pts',(1.2327422452705,-1.,-1.81817389921279));
#31234=CARTESIAN_POINT('Ctrl Pts',(1.2327422452705,1.,-1.81817389921279));
#31235=CARTESIAN_POINT('Ctrl Pts',(1.2292186489137,-1.,-1.8165508718364));
#31236=CARTESIAN_POINT('Ctrl Pts',(1.2292186489137,1.,-1.8165508718364));
#31237=CARTESIAN_POINT('Ctrl Pts',(1.2245361330495,-1.,-1.81436959210434));
#31238=CARTESIAN_POINT('Ctrl Pts',(1.2245361330495,1.,-1.81436959210434));
#31239=CARTESIAN_POINT('Ctrl Pts',(1.21870906103557,-1.,-1.81161420806656));
#31240=CARTESIAN_POINT('Ctrl Pts',(1.21870906103557,1.,-1.81161420806656));
#31241=CARTESIAN_POINT('Ctrl Pts',(1.21290815708314,-1.,-1.80882996917129));
#31242=CARTESIAN_POINT('Ctrl Pts',(1.21290815708314,1.,-1.80882996917129));
#31243=CARTESIAN_POINT('Ctrl Pts',(1.20713356605475,-1.,-1.80601678480707));
#31244=CARTESIAN_POINT('Ctrl Pts',(1.20713356605475,1.,-1.80601678480707));
#31245=CARTESIAN_POINT('Ctrl Pts',(1.20138548938974,-1.,-1.80317454838603));
#31246=CARTESIAN_POINT('Ctrl Pts',(1.20138548938974,1.,-1.80317454838603));
#31247=CARTESIAN_POINT('Ctrl Pts',(1.19566418930242,-1.,-1.80030314369879));
#31248=CARTESIAN_POINT('Ctrl Pts',(1.19566418930242,1.,-1.80030314369879));
#31249=CARTESIAN_POINT('Ctrl Pts',(1.18996997934445,-1.,-1.79740245923478));
#31250=CARTESIAN_POINT('Ctrl Pts',(1.18996997934445,1.,-1.79740245923478));
#31251=CARTESIAN_POINT('Ctrl Pts',(1.18430321697432,-1.,-1.79447240321515));
#31252=CARTESIAN_POINT('Ctrl Pts',(1.18430321697432,1.,-1.79447240321515));
#31253=CARTESIAN_POINT('Ctrl Pts',(1.17866429440809,-1.,-1.79151291552689));
#31254=CARTESIAN_POINT('Ctrl Pts',(1.17866429440809,1.,-1.79151291552689));
#31255=CARTESIAN_POINT('Ctrl Pts',(1.17305363177328,-1.,-1.78852398877617));
#31256=CARTESIAN_POINT('Ctrl Pts',(1.17305363177328,1.,-1.78852398877617));
#31257=CARTESIAN_POINT('Ctrl Pts',(1.16747166312303,-1.,-1.78550566040443));
#31258=CARTESIAN_POINT('Ctrl Pts',(1.16747166312303,1.,-1.78550566040443));
#31259=CARTESIAN_POINT('Ctrl Pts',(1.16191881298499,-1.,-1.78245795881009));
#31260=CARTESIAN_POINT('Ctrl Pts',(1.16191881298499,1.,-1.78245795881009));
#31261=CARTESIAN_POINT('Ctrl Pts',(1.15639547194698,-1.,-1.77938085564275));
#31262=CARTESIAN_POINT('Ctrl Pts',(1.15639547194698,1.,-1.77938085564275));
#31263=CARTESIAN_POINT('Ctrl Pts',(1.15090197841514,-1.,-1.7762742255701));
#31264=CARTESIAN_POINT('Ctrl Pts',(1.15090197841514,1.,-1.7762742255701));
#31265=CARTESIAN_POINT('Ctrl Pts',(1.1454385822692,-1.,-1.77313777896194));
#31266=CARTESIAN_POINT('Ctrl Pts',(1.1454385822692,1.,-1.77313777896194));
#31267=CARTESIAN_POINT('Ctrl Pts',(1.14000548336975,-1.,-1.76997111386769));
#31268=CARTESIAN_POINT('Ctrl Pts',(1.14000548336975,1.,-1.76997111386769));
#31269=CARTESIAN_POINT('Ctrl Pts',(1.1346029180462,-1.,-1.76677384551862));
#31270=CARTESIAN_POINT('Ctrl Pts',(1.1346029180462,1.,-1.76677384551862));
#31271=CARTESIAN_POINT('Ctrl Pts',(1.12923123555075,-1.,-1.7635457196617));
#31272=CARTESIAN_POINT('Ctrl Pts',(1.12923123555075,1.,-1.7635457196617));
#31273=CARTESIAN_POINT('Ctrl Pts',(1.12389096855086,-1.,-1.76028671825096));
#31274=CARTESIAN_POINT('Ctrl Pts',(1.12389096855086,1.,-1.76028671825096));
#31275=CARTESIAN_POINT('Ctrl Pts',(1.11858293216763,-1.,-1.75699720772105));
#31276=CARTESIAN_POINT('Ctrl Pts',(1.11858293216763,1.,-1.75699720772105));
#31277=CARTESIAN_POINT('Ctrl Pts',(1.11330807582551,-1.,-1.7536777209463));
#31278=CARTESIAN_POINT('Ctrl Pts',(1.11330807582551,1.,-1.7536777209463));
#31279=CARTESIAN_POINT('Ctrl Pts',(1.10806728183007,-1.,-1.7503286607592));
#31280=CARTESIAN_POINT('Ctrl Pts',(1.10806728183007,1.,-1.7503286607592));
#31281=CARTESIAN_POINT('Ctrl Pts',(1.10286118991143,-1.,-1.74695004214923));
#31282=CARTESIAN_POINT('Ctrl Pts',(1.10286118991143,1.,-1.74695004214923));
#31283=CARTESIAN_POINT('Ctrl Pts',(1.09768999241225,-1.,-1.74354119236208));
#31284=CARTESIAN_POINT('Ctrl Pts',(1.09768999241225,1.,-1.74354119236208));
#31285=CARTESIAN_POINT('Ctrl Pts',(1.09255329056493,-1.,-1.74010053962247));
#31286=CARTESIAN_POINT('Ctrl Pts',(1.09255329056493,1.,-1.74010053962247));
#31287=CARTESIAN_POINT('Ctrl Pts',(1.08745056285427,-1.,-1.73662628326091));
#31288=CARTESIAN_POINT('Ctrl Pts',(1.08745056285427,1.,-1.73662628326091));
#31289=CARTESIAN_POINT('Ctrl Pts',(1.08238162784749,-1.,-1.73311705663407));
#31290=CARTESIAN_POINT('Ctrl Pts',(1.08238162784749,1.,-1.73311705663407));
#31291=CARTESIAN_POINT('Ctrl Pts',(1.0773470373727,-1.,-1.72957248977424));
#31292=CARTESIAN_POINT('Ctrl Pts',(1.0773470373727,1.,-1.72957248977424));
#31293=CARTESIAN_POINT('Ctrl Pts',(1.07234866990252,-1.,-1.72599406198488));
#31294=CARTESIAN_POINT('Ctrl Pts',(1.07234866990252,1.,-1.72599406198488));
#31295=CARTESIAN_POINT('Ctrl Pts',(1.06738966975462,-1.,-1.72238500928453));
#31296=CARTESIAN_POINT('Ctrl Pts',(1.06738966975462,1.,-1.72238500928453));
#31297=CARTESIAN_POINT('Ctrl Pts',(1.06247324680647,-1.,-1.71874858456904));
#31298=CARTESIAN_POINT('Ctrl Pts',(1.06247324680647,1.,-1.71874858456904));
#31299=CARTESIAN_POINT('Ctrl Pts',(1.05760163192479,-1.,-1.7150865442702));
#31300=CARTESIAN_POINT('Ctrl Pts',(1.05760163192479,1.,-1.7150865442702));
#31301=CARTESIAN_POINT('Ctrl Pts',(1.05277517202855,-1.,-1.71139783543989));
#31302=CARTESIAN_POINT('Ctrl Pts',(1.05277517202855,1.,-1.71139783543989));
#31303=CARTESIAN_POINT('Ctrl Pts',(1.04799085404995,-1.,-1.70767646263649));
#31304=CARTESIAN_POINT('Ctrl Pts',(1.04799085404995,1.,-1.70767646263649));
#31305=CARTESIAN_POINT('Ctrl Pts',(1.04324363334554,-1.,-1.70391338707982));
#31306=CARTESIAN_POINT('Ctrl Pts',(1.04324363334554,1.,-1.70391338707982));
#31307=CARTESIAN_POINT('Ctrl Pts',(1.03852922490789,-1.,-1.70010052930962));
#31308=CARTESIAN_POINT('Ctrl Pts',(1.03852922490789,1.,-1.70010052930962));
#31309=CARTESIAN_POINT('Ctrl Pts',(1.03384646003588,-1.,-1.69623414782771));
#31310=CARTESIAN_POINT('Ctrl Pts',(1.03384646003588,1.,-1.69623414782771));
#31311=CARTESIAN_POINT('Ctrl Pts',(1.02919977579147,-1.,-1.69231840863458));
#31312=CARTESIAN_POINT('Ctrl Pts',(1.02919977579147,1.,-1.69231840863458));
#31313=CARTESIAN_POINT('Ctrl Pts',(1.02460180535255,-1.,-1.68836910178447));
#31314=CARTESIAN_POINT('Ctrl Pts',(1.02460180535255,1.,-1.68836910178447));
#31315=CARTESIAN_POINT('Ctrl Pts',(1.02006795074201,-1.,-1.68440578021706));
#31316=CARTESIAN_POINT('Ctrl Pts',(1.02006795074201,1.,-1.68440578021706));
#31317=CARTESIAN_POINT('Ctrl Pts',(1.01561026162773,-1.,-1.68044289894798));
#31318=CARTESIAN_POINT('Ctrl Pts',(1.01561026162773,1.,-1.68044289894798));
#31319=CARTESIAN_POINT('Ctrl Pts',(1.01123236493511,-1.,-1.67648246776464));
#31320=CARTESIAN_POINT('Ctrl Pts',(1.01123236493511,1.,-1.67648246776464));
#31321=CARTESIAN_POINT('Ctrl Pts',(1.00692206696414,-1.,-1.67250335383293));
#31322=CARTESIAN_POINT('Ctrl Pts',(1.00692206696414,1.,-1.67250335383293));
#31323=CARTESIAN_POINT('Ctrl Pts',(1.00265091003727,-1.,-1.66846059277303));
#31324=CARTESIAN_POINT('Ctrl Pts',(1.00265091003727,1.,-1.66846059277303));
#31325=CARTESIAN_POINT('Ctrl Pts',(0.998389654952757,-1.,-1.66430758030376));
#31326=CARTESIAN_POINT('Ctrl Pts',(0.998389654952757,1.,-1.66430758030376));
#31327=CARTESIAN_POINT('Ctrl Pts',(0.994121836661305,-1.,-1.66001553809947));
#31328=CARTESIAN_POINT('Ctrl Pts',(0.994121836661305,1.,-1.66001553809947));
#31329=CARTESIAN_POINT('Ctrl Pts',(0.989855627854164,-1.,-1.65559044289699));
#31330=CARTESIAN_POINT('Ctrl Pts',(0.989855627854164,1.,-1.65559044289699));
#31331=CARTESIAN_POINT('Ctrl Pts',(0.98564262292082,-1.,-1.65110016612638));
#31332=CARTESIAN_POINT('Ctrl Pts',(0.98564262292082,1.,-1.65110016612638));
#31333=CARTESIAN_POINT('Ctrl Pts',(0.981562530939489,-1.,-1.64665139190656));
#31334=CARTESIAN_POINT('Ctrl Pts',(0.981562530939489,1.,-1.64665139190656));
#31335=CARTESIAN_POINT('Ctrl Pts',(0.977689794119416,-1.,-1.64233990826687));
#31336=CARTESIAN_POINT('Ctrl Pts',(0.977689794119416,1.,-1.64233990826687));
#31337=CARTESIAN_POINT('Ctrl Pts',(0.974066058287418,-1.,-1.63820952658144));
#31338=CARTESIAN_POINT('Ctrl Pts',(0.974066058287418,1.,-1.63820952658144));
#31339=CARTESIAN_POINT('Ctrl Pts',(0.970669715997509,-1.,-1.63420665729798));
#31340=CARTESIAN_POINT('Ctrl Pts',(0.970669715997509,1.,-1.63420665729798));
#31341=CARTESIAN_POINT('Ctrl Pts',(0.967387853230345,-1.,-1.63013849959462));
#31342=CARTESIAN_POINT('Ctrl Pts',(0.967387853230345,1.,-1.63013849959462));
#31343=CARTESIAN_POINT('Ctrl Pts',(0.964046107040535,-1.,-1.62571930670187));
#31344=CARTESIAN_POINT('Ctrl Pts',(0.964046107040535,1.,-1.62571930670187));
#31345=CARTESIAN_POINT('Ctrl Pts',(0.960438326101728,-1.,-1.62061638140221));
#31346=CARTESIAN_POINT('Ctrl Pts',(0.960438326101728,1.,-1.62061638140221));
#31347=CARTESIAN_POINT('Ctrl Pts',(0.95635442292067,-1.,-1.61449324337085));
#31348=CARTESIAN_POINT('Ctrl Pts',(0.95635442292067,1.,-1.61449324337085));
#31349=CARTESIAN_POINT('Ctrl Pts',(0.951613284356035,-1.,-1.60706069896936));
#31350=CARTESIAN_POINT('Ctrl Pts',(0.951613284356035,1.,-1.60706069896936));
#31351=CARTESIAN_POINT('Ctrl Pts',(0.946078063315257,-1.,-1.59810042043673));
#31352=CARTESIAN_POINT('Ctrl Pts',(0.946078063315257,1.,-1.59810042043673));
#31353=CARTESIAN_POINT('Ctrl Pts',(0.939646377893399,-1.,-1.58744937487176));
#31354=CARTESIAN_POINT('Ctrl Pts',(0.939646377893399,1.,-1.58744937487176));
#31355=CARTESIAN_POINT('Ctrl Pts',(0.932246680108685,-1.,-1.57499388382243));
#31356=CARTESIAN_POINT('Ctrl Pts',(0.932246680108685,1.,-1.57499388382243));
#31357=CARTESIAN_POINT('Ctrl Pts',(0.923832188944341,-1.,-1.56065988578893));
#31358=CARTESIAN_POINT('Ctrl Pts',(0.923832188944341,1.,-1.56065988578893));
#31359=CARTESIAN_POINT('Ctrl Pts',(0.914375919026456,-1.,-1.54440491149498));
#31360=CARTESIAN_POINT('Ctrl Pts',(0.914375919026456,1.,-1.54440491149498));
#31361=CARTESIAN_POINT('Ctrl Pts',(0.905967409625651,-1.,-1.52984849887993));
#31362=CARTESIAN_POINT('Ctrl Pts',(0.905967409625651,1.,-1.52984849887993));
#31363=CARTESIAN_POINT('Ctrl Pts',(0.89918504748351,-1.,-1.51805569590094));
#31364=CARTESIAN_POINT('Ctrl Pts',(0.89918504748351,1.,-1.51805569590094));
#31365=CARTESIAN_POINT('Ctrl Pts',(0.894452006964543,-1.,-1.50980486806688));
#31366=CARTESIAN_POINT('Ctrl Pts',(0.894452006964543,1.,-1.50980486806688));
#31367=CARTESIAN_POINT('Ctrl Pts',(0.892032620296855,-1.,-1.5055822144029));
#31368=CARTESIAN_POINT('Ctrl Pts',(0.892032620296855,1.,-1.5055822144029));
#31369=CARTESIAN_POINT('',(1.23627494547115,1.,-1.81978687191668));
#31370=CARTESIAN_POINT('Ctrl Pts',(1.23627494547115,1.,-1.81978687191668));
#31371=CARTESIAN_POINT('Ctrl Pts',(1.23509651170476,1.,-1.81925017193666));
#31372=CARTESIAN_POINT('Ctrl Pts',(1.2327422452705,1.,-1.81817389921279));
#31373=CARTESIAN_POINT('Ctrl Pts',(1.2292186489137,1.,-1.8165508718364));
#31374=CARTESIAN_POINT('Ctrl Pts',(1.2245361330495,1.,-1.81436959210434));
#31375=CARTESIAN_POINT('Ctrl Pts',(1.21870906103557,1.,-1.81161420806656));
#31376=CARTESIAN_POINT('Ctrl Pts',(1.21290815708314,1.,-1.80882996917129));
#31377=CARTESIAN_POINT('Ctrl Pts',(1.20713356605475,1.,-1.80601678480707));
#31378=CARTESIAN_POINT('Ctrl Pts',(1.20138548938974,1.,-1.80317454838603));
#31379=CARTESIAN_POINT('Ctrl Pts',(1.19566418930242,1.,-1.80030314369879));
#31380=CARTESIAN_POINT('Ctrl Pts',(1.18996997934445,1.,-1.79740245923478));
#31381=CARTESIAN_POINT('Ctrl Pts',(1.18430321697432,1.,-1.79447240321515));
#31382=CARTESIAN_POINT('Ctrl Pts',(1.17866429440809,1.,-1.79151291552689));
#31383=CARTESIAN_POINT('Ctrl Pts',(1.17305363177328,1.,-1.78852398877617));
#31384=CARTESIAN_POINT('Ctrl Pts',(1.16747166312303,1.,-1.78550566040443));
#31385=CARTESIAN_POINT('Ctrl Pts',(1.16191881298499,1.,-1.78245795881009));
#31386=CARTESIAN_POINT('Ctrl Pts',(1.15639547194698,1.,-1.77938085564275));
#31387=CARTESIAN_POINT('Ctrl Pts',(1.15090197841514,1.,-1.7762742255701));
#31388=CARTESIAN_POINT('Ctrl Pts',(1.1454385822692,1.,-1.77313777896194));
#31389=CARTESIAN_POINT('Ctrl Pts',(1.14000548336975,1.,-1.76997111386769));
#31390=CARTESIAN_POINT('Ctrl Pts',(1.1346029180462,1.,-1.76677384551862));
#31391=CARTESIAN_POINT('Ctrl Pts',(1.12923123555075,1.,-1.7635457196617));
#31392=CARTESIAN_POINT('Ctrl Pts',(1.12389096855086,1.,-1.76028671825096));
#31393=CARTESIAN_POINT('Ctrl Pts',(1.11858293216763,1.,-1.75699720772105));
#31394=CARTESIAN_POINT('Ctrl Pts',(1.11330807582551,1.,-1.7536777209463));
#31395=CARTESIAN_POINT('Ctrl Pts',(1.10806728183007,1.,-1.7503286607592));
#31396=CARTESIAN_POINT('Ctrl Pts',(1.10286118991143,1.,-1.74695004214923));
#31397=CARTESIAN_POINT('Ctrl Pts',(1.09768999241225,1.,-1.74354119236208));
#31398=CARTESIAN_POINT('Ctrl Pts',(1.09255329056493,1.,-1.74010053962247));
#31399=CARTESIAN_POINT('Ctrl Pts',(1.08745056285427,1.,-1.73662628326091));
#31400=CARTESIAN_POINT('Ctrl Pts',(1.08238162784749,1.,-1.73311705663407));
#31401=CARTESIAN_POINT('Ctrl Pts',(1.0773470373727,1.,-1.72957248977424));
#31402=CARTESIAN_POINT('Ctrl Pts',(1.07234866990252,1.,-1.72599406198488));
#31403=CARTESIAN_POINT('Ctrl Pts',(1.06738966975462,1.,-1.72238500928453));
#31404=CARTESIAN_POINT('Ctrl Pts',(1.06247324680647,1.,-1.71874858456904));
#31405=CARTESIAN_POINT('Ctrl Pts',(1.05760163192479,1.,-1.7150865442702));
#31406=CARTESIAN_POINT('Ctrl Pts',(1.05277517202855,1.,-1.71139783543989));
#31407=CARTESIAN_POINT('Ctrl Pts',(1.04799085404995,1.,-1.70767646263649));
#31408=CARTESIAN_POINT('Ctrl Pts',(1.04324363334554,1.,-1.70391338707982));
#31409=CARTESIAN_POINT('Ctrl Pts',(1.03852922490789,1.,-1.70010052930962));
#31410=CARTESIAN_POINT('Ctrl Pts',(1.03384646003588,1.,-1.69623414782771));
#31411=CARTESIAN_POINT('Ctrl Pts',(1.02919977579147,1.,-1.69231840863458));
#31412=CARTESIAN_POINT('Ctrl Pts',(1.02460180535255,1.,-1.68836910178447));
#31413=CARTESIAN_POINT('Ctrl Pts',(1.02006795074201,1.,-1.68440578021706));
#31414=CARTESIAN_POINT('Ctrl Pts',(1.01561026162773,1.,-1.68044289894798));
#31415=CARTESIAN_POINT('Ctrl Pts',(1.01123236493511,1.,-1.67648246776464));
#31416=CARTESIAN_POINT('Ctrl Pts',(1.00692206696414,1.,-1.67250335383293));
#31417=CARTESIAN_POINT('Ctrl Pts',(1.00265091003727,1.,-1.66846059277303));
#31418=CARTESIAN_POINT('Ctrl Pts',(0.998389654952757,1.,-1.66430758030376));
#31419=CARTESIAN_POINT('Ctrl Pts',(0.994121836661305,1.,-1.66001553809947));
#31420=CARTESIAN_POINT('Ctrl Pts',(0.989855627854164,1.,-1.65559044289699));
#31421=CARTESIAN_POINT('Ctrl Pts',(0.98564262292082,1.,-1.65110016612638));
#31422=CARTESIAN_POINT('Ctrl Pts',(0.981562530939489,1.,-1.64665139190656));
#31423=CARTESIAN_POINT('Ctrl Pts',(0.977689794119416,1.,-1.64233990826687));
#31424=CARTESIAN_POINT('Ctrl Pts',(0.974066058287418,1.,-1.63820952658144));
#31425=CARTESIAN_POINT('Ctrl Pts',(0.970669715997509,1.,-1.63420665729798));
#31426=CARTESIAN_POINT('Ctrl Pts',(0.967387853230345,1.,-1.63013849959462));
#31427=CARTESIAN_POINT('Ctrl Pts',(0.964046107040535,1.,-1.62571930670187));
#31428=CARTESIAN_POINT('Ctrl Pts',(0.960438326101728,1.,-1.62061638140221));
#31429=CARTESIAN_POINT('Ctrl Pts',(0.95635442292067,1.,-1.61449324337085));
#31430=CARTESIAN_POINT('Ctrl Pts',(0.951613284356035,1.,-1.60706069896936));
#31431=CARTESIAN_POINT('Ctrl Pts',(0.946078063315257,1.,-1.59810042043673));
#31432=CARTESIAN_POINT('Ctrl Pts',(0.939646377893399,1.,-1.58744937487176));
#31433=CARTESIAN_POINT('Ctrl Pts',(0.932246680108685,1.,-1.57499388382243));
#31434=CARTESIAN_POINT('Ctrl Pts',(0.923832188944341,1.,-1.56065988578893));
#31435=CARTESIAN_POINT('Ctrl Pts',(0.914375919026456,1.,-1.54440491149498));
#31436=CARTESIAN_POINT('Ctrl Pts',(0.905967409625651,1.,-1.52984849887993));
#31437=CARTESIAN_POINT('Ctrl Pts',(0.89918504748351,1.,-1.51805569590094));
#31438=CARTESIAN_POINT('Ctrl Pts',(0.894452006964543,1.,-1.50980486806688));
#31439=CARTESIAN_POINT('Ctrl Pts',(0.892032620296855,1.,-1.5055822144029));
#31440=CARTESIAN_POINT('',(1.23627494547115,0.,-1.81978687191668));
#31441=CARTESIAN_POINT('Origin',(1.34869019493419,0.,-1.73811241238545));
#31442=CARTESIAN_POINT('',(1.34869019493419,1.,-1.73811241238545));
#31443=CARTESIAN_POINT('',(1.23627494547115,1.,-1.81978687191668));
#31444=CARTESIAN_POINT('',(1.34869019493419,0.,-1.73811241238545));
#31445=CARTESIAN_POINT('Ctrl Pts',(1.15624053661742,-1.,-1.31362392696032));
#31446=CARTESIAN_POINT('Ctrl Pts',(1.15624053661742,1.,-1.31362392696032));
#31447=CARTESIAN_POINT('Ctrl Pts',(1.15950888730809,-1.,-1.31722977216397));
#31448=CARTESIAN_POINT('Ctrl Pts',(1.15950888730809,1.,-1.31722977216397));
#31449=CARTESIAN_POINT('Ctrl Pts',(1.16589330093588,-1.,-1.32428080721772));
#31450=CARTESIAN_POINT('Ctrl Pts',(1.16589330093588,1.,-1.32428080721772));
#31451=CARTESIAN_POINT('Ctrl Pts',(1.17501305789857,-1.,-1.33437539347008));
#31452=CARTESIAN_POINT('Ctrl Pts',(1.17501305789857,1.,-1.33437539347008));
#31453=CARTESIAN_POINT('Ctrl Pts',(1.18625865667441,-1.,-1.34687054001093));
#31454=CARTESIAN_POINT('Ctrl Pts',(1.18625865667441,1.,-1.34687054001093));
#31455=CARTESIAN_POINT('Ctrl Pts',(1.1987959077932,-1.,-1.36088705043885));
#31456=CARTESIAN_POINT('Ctrl Pts',(1.1987959077932,1.,-1.36088705043885));
#31457=CARTESIAN_POINT('Ctrl Pts',(1.20982812925645,-1.,-1.37331915607905));
#31458=CARTESIAN_POINT('Ctrl Pts',(1.20982812925645,1.,-1.37331915607905));
#31459=CARTESIAN_POINT('Ctrl Pts',(1.21938737280852,-1.,-1.38420564527715));
#31460=CARTESIAN_POINT('Ctrl Pts',(1.21938737280852,1.,-1.38420564527715));
#31461=CARTESIAN_POINT('Ctrl Pts',(1.22752961899387,-1.,-1.39361389568796));
#31462=CARTESIAN_POINT('Ctrl Pts',(1.22752961899387,1.,-1.39361389568796));
#31463=CARTESIAN_POINT('Ctrl Pts',(1.23434087290423,-1.,-1.40164708206106));
#31464=CARTESIAN_POINT('Ctrl Pts',(1.23434087290423,1.,-1.40164708206106));
#31465=CARTESIAN_POINT('Ctrl Pts',(1.23994455029534,-1.,-1.40845295531283));
#31466=CARTESIAN_POINT('Ctrl Pts',(1.23994455029534,1.,-1.40845295531283));
#31467=CARTESIAN_POINT('Ctrl Pts',(1.24450600513056,-1.,-1.41422913175179));
#31468=CARTESIAN_POINT('Ctrl Pts',(1.24450600513056,1.,-1.41422913175179));
#31469=CARTESIAN_POINT('Ctrl Pts',(1.24824430986571,-1.,-1.41923722596025));
#31470=CARTESIAN_POINT('Ctrl Pts',(1.24824430986571,1.,-1.41923722596025));
#31471=CARTESIAN_POINT('Ctrl Pts',(1.2514145557001,-1.,-1.42378102115575));
#31472=CARTESIAN_POINT('Ctrl Pts',(1.2514145557001,1.,-1.42378102115575));
#31473=CARTESIAN_POINT('Ctrl Pts',(1.25426945222639,-1.,-1.42815938799387));
#31474=CARTESIAN_POINT('Ctrl Pts',(1.25426945222639,1.,-1.42815938799387));
#31475=CARTESIAN_POINT('Ctrl Pts',(1.25702687965755,-1.,-1.43262645609691));
#31476=CARTESIAN_POINT('Ctrl Pts',(1.25702687965755,1.,-1.43262645609691));
#31477=CARTESIAN_POINT('Ctrl Pts',(1.25983531012005,-1.,-1.43734919180848));
#31478=CARTESIAN_POINT('Ctrl Pts',(1.25983531012005,1.,-1.43734919180848));
#31479=CARTESIAN_POINT('Ctrl Pts',(1.26273903323858,-1.,-1.44236470511303));
#31480=CARTESIAN_POINT('Ctrl Pts',(1.26273903323858,1.,-1.44236470511303));
#31481=CARTESIAN_POINT('Ctrl Pts',(1.26570925118868,-1.,-1.44761985001662));
#31482=CARTESIAN_POINT('Ctrl Pts',(1.26570925118868,1.,-1.44761985001662));
#31483=CARTESIAN_POINT('Ctrl Pts',(1.2686778680489,-1.,-1.45301422764247));
#31484=CARTESIAN_POINT('Ctrl Pts',(1.2686778680489,1.,-1.45301422764247));
#31485=CARTESIAN_POINT('Ctrl Pts',(1.27156805265289,-1.,-1.45843906294697));
#31486=CARTESIAN_POINT('Ctrl Pts',(1.27156805265289,1.,-1.45843906294697));
#31487=CARTESIAN_POINT('Ctrl Pts',(1.27433119897822,-1.,-1.46382431332476));
#31488=CARTESIAN_POINT('Ctrl Pts',(1.27433119897822,1.,-1.46382431332476));
#31489=CARTESIAN_POINT('Ctrl Pts',(1.27696414831089,-1.,-1.46916035917133));
#31490=CARTESIAN_POINT('Ctrl Pts',(1.27696414831089,1.,-1.46916035917133));
#31491=CARTESIAN_POINT('Ctrl Pts',(1.2794891824849,-1.,-1.4744717526707));
#31492=CARTESIAN_POINT('Ctrl Pts',(1.2794891824849,1.,-1.4744717526707));
#31493=CARTESIAN_POINT('Ctrl Pts',(1.28194158939517,-1.,-1.47980070347096));
#31494=CARTESIAN_POINT('Ctrl Pts',(1.28194158939517,1.,-1.47980070347096));
#31495=CARTESIAN_POINT('Ctrl Pts',(1.28435533880201,-1.,-1.4851881711891));
#31496=CARTESIAN_POINT('Ctrl Pts',(1.28435533880201,1.,-1.4851881711891));
#31497=CARTESIAN_POINT('Ctrl Pts',(1.2867467611644,-1.,-1.4906522831278));
#31498=CARTESIAN_POINT('Ctrl Pts',(1.2867467611644,1.,-1.4906522831278));
#31499=CARTESIAN_POINT('Ctrl Pts',(1.28911506584254,-1.,-1.49618896881754));
#31500=CARTESIAN_POINT('Ctrl Pts',(1.28911506584254,1.,-1.49618896881754));
#31501=CARTESIAN_POINT('Ctrl Pts',(1.29145022885181,-1.,-1.50178230149776));
#31502=CARTESIAN_POINT('Ctrl Pts',(1.29145022885181,1.,-1.50178230149776));
#31503=CARTESIAN_POINT('Ctrl Pts',(1.29373841372842,-1.,-1.50741159078365));
#31504=CARTESIAN_POINT('Ctrl Pts',(1.29373841372842,1.,-1.50741159078365));
#31505=CARTESIAN_POINT('Ctrl Pts',(1.29596850710509,-1.,-1.51305994241402));
#31506=CARTESIAN_POINT('Ctrl Pts',(1.29596850710509,1.,-1.51305994241402));
#31507=CARTESIAN_POINT('Ctrl Pts',(1.29813791800747,-1.,-1.51872184912724));
#31508=CARTESIAN_POINT('Ctrl Pts',(1.29813791800747,1.,-1.51872184912724));
#31509=CARTESIAN_POINT('Ctrl Pts',(1.30024984366328,-1.,-1.52439957861062));
#31510=CARTESIAN_POINT('Ctrl Pts',(1.30024984366328,1.,-1.52439957861062));
#31511=CARTESIAN_POINT('Ctrl Pts',(1.30231064395568,-1.,-1.53009970283891));
#31512=CARTESIAN_POINT('Ctrl Pts',(1.30231064395568,1.,-1.53009970283891));
#31513=CARTESIAN_POINT('Ctrl Pts',(1.30432735639489,-1.,-1.53582981268977));
#31514=CARTESIAN_POINT('Ctrl Pts',(1.30432735639489,1.,-1.53582981268977));
#31515=CARTESIAN_POINT('Ctrl Pts',(1.30630475189556,-1.,-1.54159462645432));
#31516=CARTESIAN_POINT('Ctrl Pts',(1.30630475189556,1.,-1.54159462645432));
#31517=CARTESIAN_POINT('Ctrl Pts',(1.30824393907473,-1.,-1.54739413957185));
#31518=CARTESIAN_POINT('Ctrl Pts',(1.30824393907473,1.,-1.54739413957185));
#31519=CARTESIAN_POINT('Ctrl Pts',(1.31014393684222,-1.,-1.55322568759481));
#31520=CARTESIAN_POINT('Ctrl Pts',(1.31014393684222,1.,-1.55322568759481));
#31521=CARTESIAN_POINT('Ctrl Pts',(1.31200264341696,-1.,-1.55908521254821));
#31522=CARTESIAN_POINT('Ctrl Pts',(1.31200264341696,1.,-1.55908521254821));
#31523=CARTESIAN_POINT('Ctrl Pts',(1.31381795281002,-1.,-1.56496872402353));
#31524=CARTESIAN_POINT('Ctrl Pts',(1.31381795281002,1.,-1.56496872402353));
#31525=CARTESIAN_POINT('Ctrl Pts',(1.31558903860016,-1.,-1.57087397835723));
#31526=CARTESIAN_POINT('Ctrl Pts',(1.31558903860016,1.,-1.57087397835723));
#31527=CARTESIAN_POINT('Ctrl Pts',(1.31731642317187,-1.,-1.5768005650559));
#31528=CARTESIAN_POINT('Ctrl Pts',(1.31731642317187,1.,-1.5768005650559));
#31529=CARTESIAN_POINT('Ctrl Pts',(1.31900135021432,-1.,-1.58274907898834));
#31530=CARTESIAN_POINT('Ctrl Pts',(1.31900135021432,1.,-1.58274907898834));
#31531=CARTESIAN_POINT('Ctrl Pts',(1.32064537110892,-1.,-1.58872057258245));
#31532=CARTESIAN_POINT('Ctrl Pts',(1.32064537110892,1.,-1.58872057258245));
#31533=CARTESIAN_POINT('Ctrl Pts',(1.32224985747682,-1.,-1.59471591079403));
#31534=CARTESIAN_POINT('Ctrl Pts',(1.32224985747682,1.,-1.59471591079403));
#31535=CARTESIAN_POINT('Ctrl Pts',(1.32381550858256,-1.,-1.60073511858687));
#31536=CARTESIAN_POINT('Ctrl Pts',(1.32381550858256,1.,-1.60073511858687));
#31537=CARTESIAN_POINT('Ctrl Pts',(1.32534250785782,-1.,-1.60677758290954));
#31538=CARTESIAN_POINT('Ctrl Pts',(1.32534250785782,1.,-1.60677758290954));
#31539=CARTESIAN_POINT('Ctrl Pts',(1.32683074483356,-1.,-1.6128423401575));
#31540=CARTESIAN_POINT('Ctrl Pts',(1.32683074483356,1.,-1.6128423401575));
#31541=CARTESIAN_POINT('Ctrl Pts',(1.32828000610449,-1.,-1.61892832270724));
#31542=CARTESIAN_POINT('Ctrl Pts',(1.32828000610449,1.,-1.61892832270724));
#31543=CARTESIAN_POINT('Ctrl Pts',(1.3296901950568,-1.,-1.62503464209797));
#31544=CARTESIAN_POINT('Ctrl Pts',(1.3296901950568,1.,-1.62503464209797));
#31545=CARTESIAN_POINT('Ctrl Pts',(1.33106149345645,-1.,-1.63116079730923));
#31546=CARTESIAN_POINT('Ctrl Pts',(1.33106149345645,1.,-1.63116079730923));
#31547=CARTESIAN_POINT('Ctrl Pts',(1.33239425103724,-1.,-1.63730653475089));
#31548=CARTESIAN_POINT('Ctrl Pts',(1.33239425103724,1.,-1.63730653475089));
#31549=CARTESIAN_POINT('Ctrl Pts',(1.33368890676572,-1.,-1.6434717485603));
#31550=CARTESIAN_POINT('Ctrl Pts',(1.33368890676572,1.,-1.6434717485603));
#31551=CARTESIAN_POINT('Ctrl Pts',(1.33494590467993,-1.,-1.6496563728683));
#31552=CARTESIAN_POINT('Ctrl Pts',(1.33494590467993,1.,-1.6496563728683));
#31553=CARTESIAN_POINT('Ctrl Pts',(1.33616559745172,-1.,-1.65586025952593));
#31554=CARTESIAN_POINT('Ctrl Pts',(1.33616559745172,1.,-1.65586025952593));
#31555=CARTESIAN_POINT('Ctrl Pts',(1.33734820885262,-1.,-1.66208312541983));
#31556=CARTESIAN_POINT('Ctrl Pts',(1.33734820885262,1.,-1.66208312541983));
#31557=CARTESIAN_POINT('Ctrl Pts',(1.33849388654388,-1.,-1.66832460783989));
#31558=CARTESIAN_POINT('Ctrl Pts',(1.33849388654388,1.,-1.66832460783989));
#31559=CARTESIAN_POINT('Ctrl Pts',(1.3396027347034,-1.,-1.67458429426086));
#31560=CARTESIAN_POINT('Ctrl Pts',(1.3396027347034,1.,-1.67458429426086));
#31561=CARTESIAN_POINT('Ctrl Pts',(1.34067485185203,-1.,-1.68086176030362));
#31562=CARTESIAN_POINT('Ctrl Pts',(1.34067485185203,1.,-1.68086176030362));
#31563=CARTESIAN_POINT('Ctrl Pts',(1.341710374848,-1.,-1.68715660868764));
#31564=CARTESIAN_POINT('Ctrl Pts',(1.341710374848,1.,-1.68715660868764));
#31565=CARTESIAN_POINT('Ctrl Pts',(1.34270948206319,-1.,-1.6934684849687));
#31566=CARTESIAN_POINT('Ctrl Pts',(1.34270948206319,1.,-1.6934684849687));
#31567=CARTESIAN_POINT('Ctrl Pts',(1.34367237124483,-1.,-1.69979707754427));
#31568=CARTESIAN_POINT('Ctrl Pts',(1.34367237124483,1.,-1.69979707754427));
#31569=CARTESIAN_POINT('Ctrl Pts',(1.34459924533831,-1.,-1.70614212266738));
#31570=CARTESIAN_POINT('Ctrl Pts',(1.34459924533831,1.,-1.70614212266738));
#31571=CARTESIAN_POINT('Ctrl Pts',(1.34549029589416,-1.,-1.71250340686822));
#31572=CARTESIAN_POINT('Ctrl Pts',(1.34549029589416,1.,-1.71250340686822));
#31573=CARTESIAN_POINT('Ctrl Pts',(1.34634568653227,-1.,-1.7188807715049));
#31574=CARTESIAN_POINT('Ctrl Pts',(1.34634568653227,1.,-1.7188807715049));
#31575=CARTESIAN_POINT('Ctrl Pts',(1.34716554819527,-1.,-1.72527410680674));
#31576=CARTESIAN_POINT('Ctrl Pts',(1.34716554819527,1.,-1.72527410680674));
#31577=CARTESIAN_POINT('Ctrl Pts',(1.34779309152035,-1.,-1.7304014965394));
#31578=CARTESIAN_POINT('Ctrl Pts',(1.34779309152035,1.,-1.7304014965394));
#31579=CARTESIAN_POINT('Ctrl Pts',(1.34824783112887,-1.,-1.73425417885907));
#31580=CARTESIAN_POINT('Ctrl Pts',(1.34824783112887,1.,-1.73425417885907));
#31581=CARTESIAN_POINT('Ctrl Pts',(1.34854391898045,-1.,-1.73682580585691));
#31582=CARTESIAN_POINT('Ctrl Pts',(1.34854391898045,1.,-1.73682580585691));
#31583=CARTESIAN_POINT('Ctrl Pts',(1.34869019493419,-1.,-1.73811241238545));
#31584=CARTESIAN_POINT('Ctrl Pts',(1.34869019493419,1.,-1.73811241238545));
#31585=CARTESIAN_POINT('',(1.15624053661742,1.,-1.31362392696032));
#31586=CARTESIAN_POINT('Ctrl Pts',(1.15624053661742,1.,-1.31362392696032));
#31587=CARTESIAN_POINT('Ctrl Pts',(1.15950888730809,1.,-1.31722977216397));
#31588=CARTESIAN_POINT('Ctrl Pts',(1.16589330093588,1.,-1.32428080721772));
#31589=CARTESIAN_POINT('Ctrl Pts',(1.17501305789857,1.,-1.33437539347008));
#31590=CARTESIAN_POINT('Ctrl Pts',(1.18625865667441,1.,-1.34687054001093));
#31591=CARTESIAN_POINT('Ctrl Pts',(1.1987959077932,1.,-1.36088705043885));
#31592=CARTESIAN_POINT('Ctrl Pts',(1.20982812925645,1.,-1.37331915607905));
#31593=CARTESIAN_POINT('Ctrl Pts',(1.21938737280852,1.,-1.38420564527715));
#31594=CARTESIAN_POINT('Ctrl Pts',(1.22752961899387,1.,-1.39361389568796));
#31595=CARTESIAN_POINT('Ctrl Pts',(1.23434087290423,1.,-1.40164708206106));
#31596=CARTESIAN_POINT('Ctrl Pts',(1.23994455029534,1.,-1.40845295531283));
#31597=CARTESIAN_POINT('Ctrl Pts',(1.24450600513056,1.,-1.41422913175179));
#31598=CARTESIAN_POINT('Ctrl Pts',(1.24824430986571,1.,-1.41923722596025));
#31599=CARTESIAN_POINT('Ctrl Pts',(1.2514145557001,1.,-1.42378102115575));
#31600=CARTESIAN_POINT('Ctrl Pts',(1.25426945222639,1.,-1.42815938799387));
#31601=CARTESIAN_POINT('Ctrl Pts',(1.25702687965755,1.,-1.43262645609691));
#31602=CARTESIAN_POINT('Ctrl Pts',(1.25983531012005,1.,-1.43734919180848));
#31603=CARTESIAN_POINT('Ctrl Pts',(1.26273903323858,1.,-1.44236470511303));
#31604=CARTESIAN_POINT('Ctrl Pts',(1.26570925118868,1.,-1.44761985001662));
#31605=CARTESIAN_POINT('Ctrl Pts',(1.2686778680489,1.,-1.45301422764247));
#31606=CARTESIAN_POINT('Ctrl Pts',(1.27156805265289,1.,-1.45843906294697));
#31607=CARTESIAN_POINT('Ctrl Pts',(1.27433119897822,1.,-1.46382431332476));
#31608=CARTESIAN_POINT('Ctrl Pts',(1.27696414831089,1.,-1.46916035917133));
#31609=CARTESIAN_POINT('Ctrl Pts',(1.2794891824849,1.,-1.4744717526707));
#31610=CARTESIAN_POINT('Ctrl Pts',(1.28194158939517,1.,-1.47980070347096));
#31611=CARTESIAN_POINT('Ctrl Pts',(1.28435533880201,1.,-1.4851881711891));
#31612=CARTESIAN_POINT('Ctrl Pts',(1.2867467611644,1.,-1.4906522831278));
#31613=CARTESIAN_POINT('Ctrl Pts',(1.28911506584254,1.,-1.49618896881754));
#31614=CARTESIAN_POINT('Ctrl Pts',(1.29145022885181,1.,-1.50178230149776));
#31615=CARTESIAN_POINT('Ctrl Pts',(1.29373841372842,1.,-1.50741159078365));
#31616=CARTESIAN_POINT('Ctrl Pts',(1.29596850710509,1.,-1.51305994241402));
#31617=CARTESIAN_POINT('Ctrl Pts',(1.29813791800747,1.,-1.51872184912724));
#31618=CARTESIAN_POINT('Ctrl Pts',(1.30024984366328,1.,-1.52439957861062));
#31619=CARTESIAN_POINT('Ctrl Pts',(1.30231064395568,1.,-1.53009970283891));
#31620=CARTESIAN_POINT('Ctrl Pts',(1.30432735639489,1.,-1.53582981268977));
#31621=CARTESIAN_POINT('Ctrl Pts',(1.30630475189556,1.,-1.54159462645432));
#31622=CARTESIAN_POINT('Ctrl Pts',(1.30824393907473,1.,-1.54739413957185));
#31623=CARTESIAN_POINT('Ctrl Pts',(1.31014393684222,1.,-1.55322568759481));
#31624=CARTESIAN_POINT('Ctrl Pts',(1.31200264341696,1.,-1.55908521254821));
#31625=CARTESIAN_POINT('Ctrl Pts',(1.31381795281002,1.,-1.56496872402353));
#31626=CARTESIAN_POINT('Ctrl Pts',(1.31558903860016,1.,-1.57087397835723));
#31627=CARTESIAN_POINT('Ctrl Pts',(1.31731642317187,1.,-1.5768005650559));
#31628=CARTESIAN_POINT('Ctrl Pts',(1.31900135021432,1.,-1.58274907898834));
#31629=CARTESIAN_POINT('Ctrl Pts',(1.32064537110892,1.,-1.58872057258245));
#31630=CARTESIAN_POINT('Ctrl Pts',(1.32224985747682,1.,-1.59471591079403));
#31631=CARTESIAN_POINT('Ctrl Pts',(1.32381550858256,1.,-1.60073511858687));
#31632=CARTESIAN_POINT('Ctrl Pts',(1.32534250785782,1.,-1.60677758290954));
#31633=CARTESIAN_POINT('Ctrl Pts',(1.32683074483356,1.,-1.6128423401575));
#31634=CARTESIAN_POINT('Ctrl Pts',(1.32828000610449,1.,-1.61892832270724));
#31635=CARTESIAN_POINT('Ctrl Pts',(1.3296901950568,1.,-1.62503464209797));
#31636=CARTESIAN_POINT('Ctrl Pts',(1.33106149345645,1.,-1.63116079730923));
#31637=CARTESIAN_POINT('Ctrl Pts',(1.33239425103724,1.,-1.63730653475089));
#31638=CARTESIAN_POINT('Ctrl Pts',(1.33368890676572,1.,-1.6434717485603));
#31639=CARTESIAN_POINT('Ctrl Pts',(1.33494590467993,1.,-1.6496563728683));
#31640=CARTESIAN_POINT('Ctrl Pts',(1.33616559745172,1.,-1.65586025952593));
#31641=CARTESIAN_POINT('Ctrl Pts',(1.33734820885262,1.,-1.66208312541983));
#31642=CARTESIAN_POINT('Ctrl Pts',(1.33849388654388,1.,-1.66832460783989));
#31643=CARTESIAN_POINT('Ctrl Pts',(1.3396027347034,1.,-1.67458429426086));
#31644=CARTESIAN_POINT('Ctrl Pts',(1.34067485185203,1.,-1.68086176030362));
#31645=CARTESIAN_POINT('Ctrl Pts',(1.341710374848,1.,-1.68715660868764));
#31646=CARTESIAN_POINT('Ctrl Pts',(1.34270948206319,1.,-1.6934684849687));
#31647=CARTESIAN_POINT('Ctrl Pts',(1.34367237124483,1.,-1.69979707754427));
#31648=CARTESIAN_POINT('Ctrl Pts',(1.34459924533831,1.,-1.70614212266738));
#31649=CARTESIAN_POINT('Ctrl Pts',(1.34549029589416,1.,-1.71250340686822));
#31650=CARTESIAN_POINT('Ctrl Pts',(1.34634568653227,1.,-1.7188807715049));
#31651=CARTESIAN_POINT('Ctrl Pts',(1.34716554819527,1.,-1.72527410680674));
#31652=CARTESIAN_POINT('Ctrl Pts',(1.34779309152035,1.,-1.7304014965394));
#31653=CARTESIAN_POINT('Ctrl Pts',(1.34824783112887,1.,-1.73425417885907));
#31654=CARTESIAN_POINT('Ctrl Pts',(1.34854391898045,1.,-1.73682580585691));
#31655=CARTESIAN_POINT('Ctrl Pts',(1.34869019493419,1.,-1.73811241238545));
#31656=CARTESIAN_POINT('',(1.15624053661742,0.,-1.31362392696032));
#31657=CARTESIAN_POINT('Origin',(0.,0.,0.));
#31658=CARTESIAN_POINT('',(1.31362392696032,1.,-1.15624053661742));
#31659=CARTESIAN_POINT('Origin',(0.,1.,0.));
#31660=CARTESIAN_POINT('',(1.31362392696032,0.,-1.15624053661742));
#31661=CARTESIAN_POINT('Ctrl Pts',(1.73811241238545,-1.,-1.34869019493419));
#31662=CARTESIAN_POINT('Ctrl Pts',(1.73811241238545,1.,-1.34869019493419));
#31663=CARTESIAN_POINT('Ctrl Pts',(1.73682580585819,-1.,-1.34854391898145));
#31664=CARTESIAN_POINT('Ctrl Pts',(1.73682580585819,1.,-1.34854391898145));
#31665=CARTESIAN_POINT('Ctrl Pts',(1.73425417886254,-1.,-1.34824783113158));
#31666=CARTESIAN_POINT('Ctrl Pts',(1.73425417886254,1.,-1.34824783113158));
#31667=CARTESIAN_POINT('Ctrl Pts',(1.73040149654497,-1.,-1.3477930915247));
#31668=CARTESIAN_POINT('Ctrl Pts',(1.73040149654497,1.,-1.3477930915247));
#31669=CARTESIAN_POINT('Ctrl Pts',(1.72527410681298,-1.,-1.34716554820013));
#31670=CARTESIAN_POINT('Ctrl Pts',(1.72527410681298,1.,-1.34716554820013));
#31671=CARTESIAN_POINT('Ctrl Pts',(1.7188807715095,-1.,-1.34634568653586));
#31672=CARTESIAN_POINT('Ctrl Pts',(1.7188807715095,1.,-1.34634568653586));
#31673=CARTESIAN_POINT('Ctrl Pts',(1.71250340687011,-1.,-1.34549029589563));
#31674=CARTESIAN_POINT('Ctrl Pts',(1.71250340687011,1.,-1.34549029589563));
#31675=CARTESIAN_POINT('Ctrl Pts',(1.70614212266676,-1.,-1.34459924533783));
#31676=CARTESIAN_POINT('Ctrl Pts',(1.70614212266676,1.,-1.34459924533783));
#31677=CARTESIAN_POINT('Ctrl Pts',(1.69979707754221,-1.,-1.34367237124322));
#31678=CARTESIAN_POINT('Ctrl Pts',(1.69979707754221,1.,-1.34367237124322));
#31679=CARTESIAN_POINT('Ctrl Pts',(1.6934684849664,-1.,-1.34270948206139));
#31680=CARTESIAN_POINT('Ctrl Pts',(1.6934684849664,1.,-1.34270948206139));
#31681=CARTESIAN_POINT('Ctrl Pts',(1.68715660868602,-1.,-1.34171037484673));
#31682=CARTESIAN_POINT('Ctrl Pts',(1.68715660868602,1.,-1.34171037484673));
#31683=CARTESIAN_POINT('Ctrl Pts',(1.68086176030308,-1.,-1.3406748518516));
#31684=CARTESIAN_POINT('Ctrl Pts',(1.68086176030308,1.,-1.3406748518516));
#31685=CARTESIAN_POINT('Ctrl Pts',(1.67458429426126,-1.,-1.33960273470372));
#31686=CARTESIAN_POINT('Ctrl Pts',(1.67458429426126,1.,-1.33960273470372));
#31687=CARTESIAN_POINT('Ctrl Pts',(1.66832460784078,-1.,-1.33849388654458));
#31688=CARTESIAN_POINT('Ctrl Pts',(1.66832460784078,1.,-1.33849388654458));
#31689=CARTESIAN_POINT('Ctrl Pts',(1.66208312542073,-1.,-1.33734820885331));
#31690=CARTESIAN_POINT('Ctrl Pts',(1.66208312542073,1.,-1.33734820885331));
#31691=CARTESIAN_POINT('Ctrl Pts',(1.65586025952651,-1.,-1.33616559745217));
#31692=CARTESIAN_POINT('Ctrl Pts',(1.65586025952651,1.,-1.33616559745217));
#31693=CARTESIAN_POINT('Ctrl Pts',(1.64965637286843,-1.,-1.33494590468003));
#31694=CARTESIAN_POINT('Ctrl Pts',(1.64965637286843,1.,-1.33494590468003));
#31695=CARTESIAN_POINT('Ctrl Pts',(1.64347174856007,-1.,-1.33368890676554));
#31696=CARTESIAN_POINT('Ctrl Pts',(1.64347174856007,1.,-1.33368890676554));
#31697=CARTESIAN_POINT('Ctrl Pts',(1.63730653475049,-1.,-1.33239425103694));
#31698=CARTESIAN_POINT('Ctrl Pts',(1.63730653475049,1.,-1.33239425103694));
#31699=CARTESIAN_POINT('Ctrl Pts',(1.63116079730887,-1.,-1.33106149345618));
#31700=CARTESIAN_POINT('Ctrl Pts',(1.63116079730887,1.,-1.33106149345618));
#31701=CARTESIAN_POINT('Ctrl Pts',(1.62503464209777,-1.,-1.32969019505665));
#31702=CARTESIAN_POINT('Ctrl Pts',(1.62503464209777,1.,-1.32969019505665));
#31703=CARTESIAN_POINT('Ctrl Pts',(1.61892832270723,-1.,-1.32828000610448));
#31704=CARTESIAN_POINT('Ctrl Pts',(1.61892832270723,1.,-1.32828000610448));
#31705=CARTESIAN_POINT('Ctrl Pts',(1.61284234015762,-1.,-1.32683074483365));
#31706=CARTESIAN_POINT('Ctrl Pts',(1.61284234015762,1.,-1.32683074483365));
#31707=CARTESIAN_POINT('Ctrl Pts',(1.6067775829097,-1.,-1.32534250785794));
#31708=CARTESIAN_POINT('Ctrl Pts',(1.6067775829097,1.,-1.32534250785794));
#31709=CARTESIAN_POINT('Ctrl Pts',(1.600735118587,-1.,-1.32381550858266));
#31710=CARTESIAN_POINT('Ctrl Pts',(1.600735118587,1.,-1.32381550858266));
#31711=CARTESIAN_POINT('Ctrl Pts',(1.59471591079408,-1.,-1.32224985747686));
#31712=CARTESIAN_POINT('Ctrl Pts',(1.59471591079408,1.,-1.32224985747686));
#31713=CARTESIAN_POINT('Ctrl Pts',(1.58872057258244,-1.,-1.32064537110891));
#31714=CARTESIAN_POINT('Ctrl Pts',(1.58872057258244,1.,-1.32064537110891));
#31715=CARTESIAN_POINT('Ctrl Pts',(1.58274907898829,-1.,-1.31900135021428));
#31716=CARTESIAN_POINT('Ctrl Pts',(1.58274907898829,1.,-1.31900135021428));
#31717=CARTESIAN_POINT('Ctrl Pts',(1.57680056505585,-1.,-1.31731642317183));
#31718=CARTESIAN_POINT('Ctrl Pts',(1.57680056505585,1.,-1.31731642317183));
#31719=CARTESIAN_POINT('Ctrl Pts',(1.57087397835721,-1.,-1.31558903860015));
#31720=CARTESIAN_POINT('Ctrl Pts',(1.57087397835721,1.,-1.31558903860015));
#31721=CARTESIAN_POINT('Ctrl Pts',(1.56496872402352,-1.,-1.31381795281002));
#31722=CARTESIAN_POINT('Ctrl Pts',(1.56496872402352,1.,-1.31381795281002));
#31723=CARTESIAN_POINT('Ctrl Pts',(1.55908521254822,-1.,-1.31200264341696));
#31724=CARTESIAN_POINT('Ctrl Pts',(1.55908521254822,1.,-1.31200264341696));
#31725=CARTESIAN_POINT('Ctrl Pts',(1.55322568759481,-1.,-1.31014393684221));
#31726=CARTESIAN_POINT('Ctrl Pts',(1.55322568759481,1.,-1.31014393684221));
#31727=CARTESIAN_POINT('Ctrl Pts',(1.54739413957183,-1.,-1.30824393907471));
#31728=CARTESIAN_POINT('Ctrl Pts',(1.54739413957183,1.,-1.30824393907471));
#31729=CARTESIAN_POINT('Ctrl Pts',(1.54159462645428,-1.,-1.30630475189553));
#31730=CARTESIAN_POINT('Ctrl Pts',(1.54159462645428,1.,-1.30630475189553));
#31731=CARTESIAN_POINT('Ctrl Pts',(1.53582981268976,-1.,-1.30432735639487));
#31732=CARTESIAN_POINT('Ctrl Pts',(1.53582981268976,1.,-1.30432735639487));
#31733=CARTESIAN_POINT('Ctrl Pts',(1.53009970283893,-1.,-1.3023106439557));
#31734=CARTESIAN_POINT('Ctrl Pts',(1.53009970283893,1.,-1.3023106439557));
#31735=CARTESIAN_POINT('Ctrl Pts',(1.5243995786107,-1.,-1.30024984366334));
#31736=CARTESIAN_POINT('Ctrl Pts',(1.5243995786107,1.,-1.30024984366334));
#31737=CARTESIAN_POINT('Ctrl Pts',(1.51872184912735,-1.,-1.29813791800757));
#31738=CARTESIAN_POINT('Ctrl Pts',(1.51872184912735,1.,-1.29813791800757));
#31739=CARTESIAN_POINT('Ctrl Pts',(1.51305994241412,-1.,-1.29596850710518));
#31740=CARTESIAN_POINT('Ctrl Pts',(1.51305994241412,1.,-1.29596850710518));
#31741=CARTESIAN_POINT('Ctrl Pts',(1.50741159078367,-1.,-1.29373841372843));
#31742=CARTESIAN_POINT('Ctrl Pts',(1.50741159078367,1.,-1.29373841372843));
#31743=CARTESIAN_POINT('Ctrl Pts',(1.50178230149764,-1.,-1.29145022885171));
#31744=CARTESIAN_POINT('Ctrl Pts',(1.50178230149764,1.,-1.29145022885171));
#31745=CARTESIAN_POINT('Ctrl Pts',(1.49618896881729,-1.,-1.28911506584232));
#31746=CARTESIAN_POINT('Ctrl Pts',(1.49618896881729,1.,-1.28911506584232));
#31747=CARTESIAN_POINT('Ctrl Pts',(1.4906522831275,-1.,-1.28674676116415));
#31748=CARTESIAN_POINT('Ctrl Pts',(1.4906522831275,1.,-1.28674676116415));
#31749=CARTESIAN_POINT('Ctrl Pts',(1.48518817118891,-1.,-1.28435533880184));
#31750=CARTESIAN_POINT('Ctrl Pts',(1.48518817118891,1.,-1.28435533880184));
#31751=CARTESIAN_POINT('Ctrl Pts',(1.47980070347102,-1.,-1.28194158939522));
#31752=CARTESIAN_POINT('Ctrl Pts',(1.47980070347102,1.,-1.28194158939522));
#31753=CARTESIAN_POINT('Ctrl Pts',(1.4744717526711,-1.,-1.27948918248524));
#31754=CARTESIAN_POINT('Ctrl Pts',(1.4744717526711,1.,-1.27948918248524));
#31755=CARTESIAN_POINT('Ctrl Pts',(1.46916035917197,-1.,-1.27696414831144));
#31756=CARTESIAN_POINT('Ctrl Pts',(1.46916035917197,1.,-1.27696414831144));
#31757=CARTESIAN_POINT('Ctrl Pts',(1.4638243133254,-1.,-1.27433119897877));
#31758=CARTESIAN_POINT('Ctrl Pts',(1.4638243133254,1.,-1.27433119897877));
#31759=CARTESIAN_POINT('Ctrl Pts',(1.45843906294725,-1.,-1.27156805265312));
#31760=CARTESIAN_POINT('Ctrl Pts',(1.45843906294725,1.,-1.27156805265312));
#31761=CARTESIAN_POINT('Ctrl Pts',(1.45301422764205,-1.,-1.26867786804854));
#31762=CARTESIAN_POINT('Ctrl Pts',(1.45301422764205,1.,-1.26867786804854));
#31763=CARTESIAN_POINT('Ctrl Pts',(1.44761985001544,-1.,-1.26570925118767));
#31764=CARTESIAN_POINT('Ctrl Pts',(1.44761985001544,1.,-1.26570925118767));
#31765=CARTESIAN_POINT('Ctrl Pts',(1.44236470511145,-1.,-1.26273903323723));
#31766=CARTESIAN_POINT('Ctrl Pts',(1.44236470511145,1.,-1.26273903323723));
#31767=CARTESIAN_POINT('Ctrl Pts',(1.43734919180719,-1.,-1.25983531011894));
#31768=CARTESIAN_POINT('Ctrl Pts',(1.43734919180719,1.,-1.25983531011894));
#31769=CARTESIAN_POINT('Ctrl Pts',(1.43262645609679,-1.,-1.25702687965744));
#31770=CARTESIAN_POINT('Ctrl Pts',(1.43262645609679,1.,-1.25702687965744));
#31771=CARTESIAN_POINT('Ctrl Pts',(1.42815938799555,-1.,-1.25426945222783));
#31772=CARTESIAN_POINT('Ctrl Pts',(1.42815938799555,1.,-1.25426945222783));
#31773=CARTESIAN_POINT('Ctrl Pts',(1.42378102115911,-1.,-1.25141455570299));
#31774=CARTESIAN_POINT('Ctrl Pts',(1.42378102115911,1.,-1.25141455570299));
#31775=CARTESIAN_POINT('Ctrl Pts',(1.41923722596421,-1.,-1.24824430986911));
#31776=CARTESIAN_POINT('Ctrl Pts',(1.41923722596421,1.,-1.24824430986911));
#31777=CARTESIAN_POINT('Ctrl Pts',(1.41422913175437,-1.,-1.24450600513278));
#31778=CARTESIAN_POINT('Ctrl Pts',(1.41422913175437,1.,-1.24450600513278));
#31779=CARTESIAN_POINT('Ctrl Pts',(1.40845295531151,-1.,-1.23994455029421));
#31780=CARTESIAN_POINT('Ctrl Pts',(1.40845295531151,1.,-1.23994455029421));
#31781=CARTESIAN_POINT('Ctrl Pts',(1.40164708205345,-1.,-1.23434087289768));
#31782=CARTESIAN_POINT('Ctrl Pts',(1.40164708205345,1.,-1.23434087289768));
#31783=CARTESIAN_POINT('Ctrl Pts',(1.39361389567257,-1.,-1.22752961898063));
#31784=CARTESIAN_POINT('Ctrl Pts',(1.39361389567257,1.,-1.22752961898063));
#31785=CARTESIAN_POINT('Ctrl Pts',(1.38420564525391,-1.,-1.21938737278853));
#31786=CARTESIAN_POINT('Ctrl Pts',(1.38420564525391,1.,-1.21938737278853));
#31787=CARTESIAN_POINT('Ctrl Pts',(1.37331915604962,-1.,-1.20982812923113));
#31788=CARTESIAN_POINT('Ctrl Pts',(1.37331915604962,1.,-1.20982812923113));
#31789=CARTESIAN_POINT('Ctrl Pts',(1.36088705040677,-1.,-1.1987959077656));
#31790=CARTESIAN_POINT('Ctrl Pts',(1.36088705040677,1.,-1.1987959077656));
#31791=CARTESIAN_POINT('Ctrl Pts',(1.34687053998157,-1.,-1.18625865664915));
#31792=CARTESIAN_POINT('Ctrl Pts',(1.34687053998157,1.,-1.18625865664915));
#31793=CARTESIAN_POINT('Ctrl Pts',(1.33437539344842,-1.,-1.17501305787994));
#31794=CARTESIAN_POINT('Ctrl Pts',(1.33437539344842,1.,-1.17501305787994));
#31795=CARTESIAN_POINT('Ctrl Pts',(1.32428080720544,-1.,-1.16589330092532));
#31796=CARTESIAN_POINT('Ctrl Pts',(1.32428080720544,1.,-1.16589330092532));
#31797=CARTESIAN_POINT('Ctrl Pts',(1.3172297721596,-1.,-1.15950888730433));
#31798=CARTESIAN_POINT('Ctrl Pts',(1.3172297721596,1.,-1.15950888730433));
#31799=CARTESIAN_POINT('Ctrl Pts',(1.31362392696032,-1.,-1.15624053661742));
#31800=CARTESIAN_POINT('Ctrl Pts',(1.31362392696032,1.,-1.15624053661742));
#31801=CARTESIAN_POINT('',(1.73811241238545,1.,-1.34869019493419));
#31802=CARTESIAN_POINT('Ctrl Pts',(1.73811241238545,1.,-1.34869019493419));
#31803=CARTESIAN_POINT('Ctrl Pts',(1.73682580585819,1.,-1.34854391898145));
#31804=CARTESIAN_POINT('Ctrl Pts',(1.73425417886254,1.,-1.34824783113158));
#31805=CARTESIAN_POINT('Ctrl Pts',(1.73040149654497,1.,-1.3477930915247));
#31806=CARTESIAN_POINT('Ctrl Pts',(1.72527410681298,1.,-1.34716554820013));
#31807=CARTESIAN_POINT('Ctrl Pts',(1.7188807715095,1.,-1.34634568653586));
#31808=CARTESIAN_POINT('Ctrl Pts',(1.71250340687011,1.,-1.34549029589563));
#31809=CARTESIAN_POINT('Ctrl Pts',(1.70614212266676,1.,-1.34459924533783));
#31810=CARTESIAN_POINT('Ctrl Pts',(1.69979707754221,1.,-1.34367237124322));
#31811=CARTESIAN_POINT('Ctrl Pts',(1.6934684849664,1.,-1.34270948206139));
#31812=CARTESIAN_POINT('Ctrl Pts',(1.68715660868602,1.,-1.34171037484673));
#31813=CARTESIAN_POINT('Ctrl Pts',(1.68086176030308,1.,-1.3406748518516));
#31814=CARTESIAN_POINT('Ctrl Pts',(1.67458429426126,1.,-1.33960273470372));
#31815=CARTESIAN_POINT('Ctrl Pts',(1.66832460784078,1.,-1.33849388654458));
#31816=CARTESIAN_POINT('Ctrl Pts',(1.66208312542073,1.,-1.33734820885331));
#31817=CARTESIAN_POINT('Ctrl Pts',(1.65586025952651,1.,-1.33616559745217));
#31818=CARTESIAN_POINT('Ctrl Pts',(1.64965637286843,1.,-1.33494590468003));
#31819=CARTESIAN_POINT('Ctrl Pts',(1.64347174856007,1.,-1.33368890676554));
#31820=CARTESIAN_POINT('Ctrl Pts',(1.63730653475049,1.,-1.33239425103694));
#31821=CARTESIAN_POINT('Ctrl Pts',(1.63116079730887,1.,-1.33106149345618));
#31822=CARTESIAN_POINT('Ctrl Pts',(1.62503464209777,1.,-1.32969019505665));
#31823=CARTESIAN_POINT('Ctrl Pts',(1.61892832270723,1.,-1.32828000610448));
#31824=CARTESIAN_POINT('Ctrl Pts',(1.61284234015762,1.,-1.32683074483365));
#31825=CARTESIAN_POINT('Ctrl Pts',(1.6067775829097,1.,-1.32534250785794));
#31826=CARTESIAN_POINT('Ctrl Pts',(1.600735118587,1.,-1.32381550858266));
#31827=CARTESIAN_POINT('Ctrl Pts',(1.59471591079408,1.,-1.32224985747686));
#31828=CARTESIAN_POINT('Ctrl Pts',(1.58872057258244,1.,-1.32064537110891));
#31829=CARTESIAN_POINT('Ctrl Pts',(1.58274907898829,1.,-1.31900135021428));
#31830=CARTESIAN_POINT('Ctrl Pts',(1.57680056505585,1.,-1.31731642317183));
#31831=CARTESIAN_POINT('Ctrl Pts',(1.57087397835721,1.,-1.31558903860015));
#31832=CARTESIAN_POINT('Ctrl Pts',(1.56496872402352,1.,-1.31381795281002));
#31833=CARTESIAN_POINT('Ctrl Pts',(1.55908521254822,1.,-1.31200264341696));
#31834=CARTESIAN_POINT('Ctrl Pts',(1.55322568759481,1.,-1.31014393684221));
#31835=CARTESIAN_POINT('Ctrl Pts',(1.54739413957183,1.,-1.30824393907471));
#31836=CARTESIAN_POINT('Ctrl Pts',(1.54159462645428,1.,-1.30630475189553));
#31837=CARTESIAN_POINT('Ctrl Pts',(1.53582981268976,1.,-1.30432735639487));
#31838=CARTESIAN_POINT('Ctrl Pts',(1.53009970283893,1.,-1.3023106439557));
#31839=CARTESIAN_POINT('Ctrl Pts',(1.5243995786107,1.,-1.30024984366334));
#31840=CARTESIAN_POINT('Ctrl Pts',(1.51872184912735,1.,-1.29813791800757));
#31841=CARTESIAN_POINT('Ctrl Pts',(1.51305994241412,1.,-1.29596850710518));
#31842=CARTESIAN_POINT('Ctrl Pts',(1.50741159078367,1.,-1.29373841372843));
#31843=CARTESIAN_POINT('Ctrl Pts',(1.50178230149764,1.,-1.29145022885171));
#31844=CARTESIAN_POINT('Ctrl Pts',(1.49618896881729,1.,-1.28911506584232));
#31845=CARTESIAN_POINT('Ctrl Pts',(1.4906522831275,1.,-1.28674676116415));
#31846=CARTESIAN_POINT('Ctrl Pts',(1.48518817118891,1.,-1.28435533880184));
#31847=CARTESIAN_POINT('Ctrl Pts',(1.47980070347102,1.,-1.28194158939522));
#31848=CARTESIAN_POINT('Ctrl Pts',(1.4744717526711,1.,-1.27948918248524));
#31849=CARTESIAN_POINT('Ctrl Pts',(1.46916035917197,1.,-1.27696414831144));
#31850=CARTESIAN_POINT('Ctrl Pts',(1.4638243133254,1.,-1.27433119897877));
#31851=CARTESIAN_POINT('Ctrl Pts',(1.45843906294725,1.,-1.27156805265312));
#31852=CARTESIAN_POINT('Ctrl Pts',(1.45301422764205,1.,-1.26867786804854));
#31853=CARTESIAN_POINT('Ctrl Pts',(1.44761985001544,1.,-1.26570925118767));
#31854=CARTESIAN_POINT('Ctrl Pts',(1.44236470511145,1.,-1.26273903323723));
#31855=CARTESIAN_POINT('Ctrl Pts',(1.43734919180719,1.,-1.25983531011894));
#31856=CARTESIAN_POINT('Ctrl Pts',(1.43262645609679,1.,-1.25702687965744));
#31857=CARTESIAN_POINT('Ctrl Pts',(1.42815938799555,1.,-1.25426945222783));
#31858=CARTESIAN_POINT('Ctrl Pts',(1.42378102115911,1.,-1.25141455570299));
#31859=CARTESIAN_POINT('Ctrl Pts',(1.41923722596421,1.,-1.24824430986911));
#31860=CARTESIAN_POINT('Ctrl Pts',(1.41422913175437,1.,-1.24450600513278));
#31861=CARTESIAN_POINT('Ctrl Pts',(1.40845295531151,1.,-1.23994455029421));
#31862=CARTESIAN_POINT('Ctrl Pts',(1.40164708205345,1.,-1.23434087289768));
#31863=CARTESIAN_POINT('Ctrl Pts',(1.39361389567257,1.,-1.22752961898063));
#31864=CARTESIAN_POINT('Ctrl Pts',(1.38420564525391,1.,-1.21938737278853));
#31865=CARTESIAN_POINT('Ctrl Pts',(1.37331915604962,1.,-1.20982812923113));
#31866=CARTESIAN_POINT('Ctrl Pts',(1.36088705040677,1.,-1.1987959077656));
#31867=CARTESIAN_POINT('Ctrl Pts',(1.34687053998157,1.,-1.18625865664915));
#31868=CARTESIAN_POINT('Ctrl Pts',(1.33437539344842,1.,-1.17501305787994));
#31869=CARTESIAN_POINT('Ctrl Pts',(1.32428080720544,1.,-1.16589330092532));
#31870=CARTESIAN_POINT('Ctrl Pts',(1.3172297721596,1.,-1.15950888730433));
#31871=CARTESIAN_POINT('Ctrl Pts',(1.31362392696032,1.,-1.15624053661742));
#31872=CARTESIAN_POINT('',(1.73811241238545,0.,-1.34869019493419));
#31873=CARTESIAN_POINT('Origin',(1.81978687191668,0.,-1.23627494547115));
#31874=CARTESIAN_POINT('',(1.81978687191668,1.,-1.23627494547115));
#31875=CARTESIAN_POINT('',(1.73811241238545,1.,-1.34869019493419));
#31876=CARTESIAN_POINT('',(1.81978687191668,0.,-1.23627494547115));
#31877=CARTESIAN_POINT('Ctrl Pts',(1.5055822144029,-1.,-0.892032620296855));
#31878=CARTESIAN_POINT('Ctrl Pts',(1.5055822144029,1.,-0.892032620296855));
#31879=CARTESIAN_POINT('Ctrl Pts',(1.50980486807181,-1.,-0.894452006967538));
#31880=CARTESIAN_POINT('Ctrl Pts',(1.50980486807181,1.,-0.894452006967538));
#31881=CARTESIAN_POINT('Ctrl Pts',(1.51805569591479,-1.,-0.89918504749193));
#31882=CARTESIAN_POINT('Ctrl Pts',(1.51805569591479,1.,-0.89918504749193));
#31883=CARTESIAN_POINT('Ctrl Pts',(1.52984849890434,-1.,-0.905967409640499));
#31884=CARTESIAN_POINT('Ctrl Pts',(1.52984849890434,1.,-0.905967409640499));
#31885=CARTESIAN_POINT('Ctrl Pts',(1.54440491152807,-1.,-0.91437591904658));
#31886=CARTESIAN_POINT('Ctrl Pts',(1.54440491152807,1.,-0.91437591904658));
#31887=CARTESIAN_POINT('Ctrl Pts',(1.56065988582509,-1.,-0.923832188966322));
#31888=CARTESIAN_POINT('Ctrl Pts',(1.56065988582509,1.,-0.923832188966322));
#31889=CARTESIAN_POINT('Ctrl Pts',(1.57499388385561,-1.,-0.932246680128849));
#31890=CARTESIAN_POINT('Ctrl Pts',(1.57499388385561,1.,-0.932246680128849));
#31891=CARTESIAN_POINT('Ctrl Pts',(1.58744937489796,-1.,-0.939646377909319));
#31892=CARTESIAN_POINT('Ctrl Pts',(1.58744937489796,1.,-0.939646377909319));
#31893=CARTESIAN_POINT('Ctrl Pts',(1.59810042045408,-1.,-0.946078063325796));
#31894=CARTESIAN_POINT('Ctrl Pts',(1.59810042045408,1.,-0.946078063325796));
#31895=CARTESIAN_POINT('Ctrl Pts',(1.60706069897794,-1.,-0.951613284361248));
#31896=CARTESIAN_POINT('Ctrl Pts',(1.60706069897794,1.,-0.951613284361248));
#31897=CARTESIAN_POINT('Ctrl Pts',(1.61449324337233,-1.,-0.956354422921573));
#31898=CARTESIAN_POINT('Ctrl Pts',(1.61449324337233,1.,-0.956354422921573));
#31899=CARTESIAN_POINT('Ctrl Pts',(1.62061638139929,-1.,-0.960438326099958));
#31900=CARTESIAN_POINT('Ctrl Pts',(1.62061638139929,1.,-0.960438326099958));
#31901=CARTESIAN_POINT('Ctrl Pts',(1.6257193066974,-1.,-0.964046107037821));
#31902=CARTESIAN_POINT('Ctrl Pts',(1.6257193066974,1.,-0.964046107037821));
#31903=CARTESIAN_POINT('Ctrl Pts',(1.63013849959083,-1.,-0.967387853228041));
#31904=CARTESIAN_POINT('Ctrl Pts',(1.63013849959083,1.,-0.967387853228041));
#31905=CARTESIAN_POINT('Ctrl Pts',(1.63420665729609,-1.,-0.970669715996356));
#31906=CARTESIAN_POINT('Ctrl Pts',(1.63420665729609,1.,-0.970669715996356));
#31907=CARTESIAN_POINT('Ctrl Pts',(1.63820952658157,-1.,-0.974066058287501));
#31908=CARTESIAN_POINT('Ctrl Pts',(1.63820952658157,1.,-0.974066058287501));
#31909=CARTESIAN_POINT('Ctrl Pts',(1.64233990826831,-1.,-0.977689794120297));
#31910=CARTESIAN_POINT('Ctrl Pts',(1.64233990826831,1.,-0.977689794120297));
#31911=CARTESIAN_POINT('Ctrl Pts',(1.64665139190834,-1.,-0.981562530940574));
#31912=CARTESIAN_POINT('Ctrl Pts',(1.64665139190834,1.,-0.981562530940574));
#31913=CARTESIAN_POINT('Ctrl Pts',(1.6511001661277,-1.,-0.985642622921626));
#31914=CARTESIAN_POINT('Ctrl Pts',(1.6511001661277,1.,-0.985642622921626));
#31915=CARTESIAN_POINT('Ctrl Pts',(1.65559044289746,-1.,-0.98985562785445));
#31916=CARTESIAN_POINT('Ctrl Pts',(1.65559044289746,1.,-0.98985562785445));
#31917=CARTESIAN_POINT('Ctrl Pts',(1.66001553809916,-1.,-0.994121836661116));
#31918=CARTESIAN_POINT('Ctrl Pts',(1.66001553809916,1.,-0.994121836661116));
#31919=CARTESIAN_POINT('Ctrl Pts',(1.66430758030304,-1.,-0.998389654952317));
#31920=CARTESIAN_POINT('Ctrl Pts',(1.66430758030304,1.,-0.998389654952317));
#31921=CARTESIAN_POINT('Ctrl Pts',(1.66846059277231,-1.,-1.00265091003682));
#31922=CARTESIAN_POINT('Ctrl Pts',(1.66846059277231,1.,-1.00265091003682));
#31923=CARTESIAN_POINT('Ctrl Pts',(1.67250335383248,-1.,-1.00692206696387));
#31924=CARTESIAN_POINT('Ctrl Pts',(1.67250335383248,1.,-1.00692206696387));
#31925=CARTESIAN_POINT('Ctrl Pts',(1.67648246776457,-1.,-1.01123236493507));
#31926=CARTESIAN_POINT('Ctrl Pts',(1.67648246776457,1.,-1.01123236493507));
#31927=CARTESIAN_POINT('Ctrl Pts',(1.6804428989482,-1.,-1.01561026162787));
#31928=CARTESIAN_POINT('Ctrl Pts',(1.6804428989482,1.,-1.01561026162787));
#31929=CARTESIAN_POINT('Ctrl Pts',(1.68440578021739,-1.,-1.02006795074222));
#31930=CARTESIAN_POINT('Ctrl Pts',(1.68440578021739,1.,-1.02006795074222));
#31931=CARTESIAN_POINT('Ctrl Pts',(1.68836910178475,-1.,-1.02460180535272));
#31932=CARTESIAN_POINT('Ctrl Pts',(1.68836910178475,1.,-1.02460180535272));
#31933=CARTESIAN_POINT('Ctrl Pts',(1.69231840863471,-1.,-1.02919977579155));
#31934=CARTESIAN_POINT('Ctrl Pts',(1.69231840863471,1.,-1.02919977579155));
#31935=CARTESIAN_POINT('Ctrl Pts',(1.69623414782769,-1.,-1.03384646003587));
#31936=CARTESIAN_POINT('Ctrl Pts',(1.69623414782769,1.,-1.03384646003587));
#31937=CARTESIAN_POINT('Ctrl Pts',(1.70010052930951,-1.,-1.03852922490782));
#31938=CARTESIAN_POINT('Ctrl Pts',(1.70010052930951,1.,-1.03852922490782));
#31939=CARTESIAN_POINT('Ctrl Pts',(1.70391338707969,-1.,-1.04324363334546));
#31940=CARTESIAN_POINT('Ctrl Pts',(1.70391338707969,1.,-1.04324363334546));
#31941=CARTESIAN_POINT('Ctrl Pts',(1.70767646263641,-1.,-1.0479908540499));
#31942=CARTESIAN_POINT('Ctrl Pts',(1.70767646263641,1.,-1.0479908540499));
#31943=CARTESIAN_POINT('Ctrl Pts',(1.71139783543986,-1.,-1.05277517202854));
#31944=CARTESIAN_POINT('Ctrl Pts',(1.71139783543986,1.,-1.05277517202854));
#31945=CARTESIAN_POINT('Ctrl Pts',(1.71508654427022,-1.,-1.05760163192481));
#31946=CARTESIAN_POINT('Ctrl Pts',(1.71508654427022,1.,-1.05760163192481));
#31947=CARTESIAN_POINT('Ctrl Pts',(1.71874858456908,-1.,-1.0624732468065));
#31948=CARTESIAN_POINT('Ctrl Pts',(1.71874858456908,1.,-1.0624732468065));
#31949=CARTESIAN_POINT('Ctrl Pts',(1.72238500928456,-1.,-1.06738966975463));
#31950=CARTESIAN_POINT('Ctrl Pts',(1.72238500928456,1.,-1.06738966975463));
#31951=CARTESIAN_POINT('Ctrl Pts',(1.72599406198489,-1.,-1.07234866990252));
#31952=CARTESIAN_POINT('Ctrl Pts',(1.72599406198489,1.,-1.07234866990252));
#31953=CARTESIAN_POINT('Ctrl Pts',(1.72957248977424,-1.,-1.0773470373727));
#31954=CARTESIAN_POINT('Ctrl Pts',(1.72957248977424,1.,-1.0773470373727));
#31955=CARTESIAN_POINT('Ctrl Pts',(1.73311705663407,-1.,-1.08238162784749));
#31956=CARTESIAN_POINT('Ctrl Pts',(1.73311705663407,1.,-1.08238162784749));
#31957=CARTESIAN_POINT('Ctrl Pts',(1.73662628326093,-1.,-1.08745056285429));
#31958=CARTESIAN_POINT('Ctrl Pts',(1.73662628326093,1.,-1.08745056285429));
#31959=CARTESIAN_POINT('Ctrl Pts',(1.74010053962252,-1.,-1.09255329056496));
#31960=CARTESIAN_POINT('Ctrl Pts',(1.74010053962252,1.,-1.09255329056496));
#31961=CARTESIAN_POINT('Ctrl Pts',(1.74354119236212,-1.,-1.09768999241229));
#31962=CARTESIAN_POINT('Ctrl Pts',(1.74354119236212,1.,-1.09768999241229));
#31963=CARTESIAN_POINT('Ctrl Pts',(1.74695004214924,-1.,-1.10286118991144));
#31964=CARTESIAN_POINT('Ctrl Pts',(1.74695004214924,1.,-1.10286118991144));
#31965=CARTESIAN_POINT('Ctrl Pts',(1.75032866075914,-1.,-1.10806728183003));
#31966=CARTESIAN_POINT('Ctrl Pts',(1.75032866075914,1.,-1.10806728183003));
#31967=CARTESIAN_POINT('Ctrl Pts',(1.75367772094617,-1.,-1.11330807582542));
#31968=CARTESIAN_POINT('Ctrl Pts',(1.75367772094617,1.,-1.11330807582542));
#31969=CARTESIAN_POINT('Ctrl Pts',(1.75699720772089,-1.,-1.11858293216752));
#31970=CARTESIAN_POINT('Ctrl Pts',(1.75699720772089,1.,-1.11858293216752));
#31971=CARTESIAN_POINT('Ctrl Pts',(1.76028671825084,-1.,-1.12389096855078));
#31972=CARTESIAN_POINT('Ctrl Pts',(1.76028671825084,1.,-1.12389096855078));
#31973=CARTESIAN_POINT('Ctrl Pts',(1.76354571966171,-1.,-1.12923123555076));
#31974=CARTESIAN_POINT('Ctrl Pts',(1.76354571966171,1.,-1.12923123555076));
#31975=CARTESIAN_POINT('Ctrl Pts',(1.76677384551883,-1.,-1.13460291804635));
#31976=CARTESIAN_POINT('Ctrl Pts',(1.76677384551883,1.,-1.13460291804635));
#31977=CARTESIAN_POINT('Ctrl Pts',(1.76997111386806,-1.,-1.14000548337));
#31978=CARTESIAN_POINT('Ctrl Pts',(1.76997111386806,1.,-1.14000548337));
#31979=CARTESIAN_POINT('Ctrl Pts',(1.77313777896234,-1.,-1.14543858226948));
#31980=CARTESIAN_POINT('Ctrl Pts',(1.77313777896234,1.,-1.14543858226948));
#31981=CARTESIAN_POINT('Ctrl Pts',(1.77627422557034,-1.,-1.15090197841531));
#31982=CARTESIAN_POINT('Ctrl Pts',(1.77627422557034,1.,-1.15090197841531));
#31983=CARTESIAN_POINT('Ctrl Pts',(1.77938085564261,-1.,-1.15639547194689));
#31984=CARTESIAN_POINT('Ctrl Pts',(1.77938085564261,1.,-1.15639547194689));
#31985=CARTESIAN_POINT('Ctrl Pts',(1.78245795880949,-1.,-1.16191881298458));
#31986=CARTESIAN_POINT('Ctrl Pts',(1.78245795880949,1.,-1.16191881298458));
#31987=CARTESIAN_POINT('Ctrl Pts',(1.78550566040349,-1.,-1.16747166312239));
#31988=CARTESIAN_POINT('Ctrl Pts',(1.78550566040349,1.,-1.16747166312239));
#31989=CARTESIAN_POINT('Ctrl Pts',(1.78852398877523,-1.,-1.17305363177265));
#31990=CARTESIAN_POINT('Ctrl Pts',(1.78852398877523,1.,-1.17305363177265));
#31991=CARTESIAN_POINT('Ctrl Pts',(1.79151291552646,-1.,-1.17866429440781));
#31992=CARTESIAN_POINT('Ctrl Pts',(1.79151291552646,1.,-1.17866429440781));
#31993=CARTESIAN_POINT('Ctrl Pts',(1.79447240321572,-1.,-1.18430321697471));
#31994=CARTESIAN_POINT('Ctrl Pts',(1.79447240321572,1.,-1.18430321697471));
#31995=CARTESIAN_POINT('Ctrl Pts',(1.79740245923649,-1.,-1.1899699793456));
#31996=CARTESIAN_POINT('Ctrl Pts',(1.79740245923649,1.,-1.1899699793456));
#31997=CARTESIAN_POINT('Ctrl Pts',(1.80030314370121,-1.,-1.19566418930405));
#31998=CARTESIAN_POINT('Ctrl Pts',(1.80030314370121,1.,-1.19566418930405));
#31999=CARTESIAN_POINT('Ctrl Pts',(1.8031745483882,-1.,-1.2013854893912));
#32000=CARTESIAN_POINT('Ctrl Pts',(1.8031745483882,1.,-1.2013854893912));
#32001=CARTESIAN_POINT('Ctrl Pts',(1.80601678480772,-1.,-1.20713356605519));
#32002=CARTESIAN_POINT('Ctrl Pts',(1.80601678480772,1.,-1.20713356605519));
#32003=CARTESIAN_POINT('Ctrl Pts',(1.80882996916931,-1.,-1.2129081570818));
#32004=CARTESIAN_POINT('Ctrl Pts',(1.80882996916931,1.,-1.2129081570818));
#32005=CARTESIAN_POINT('Ctrl Pts',(1.81161420806172,-1.,-1.2187090610323));
#32006=CARTESIAN_POINT('Ctrl Pts',(1.81161420806172,1.,-1.2187090610323));
#32007=CARTESIAN_POINT('Ctrl Pts',(1.81436959209778,-1.,-1.22453613304507));
#32008=CARTESIAN_POINT('Ctrl Pts',(1.81436959209778,1.,-1.22453613304507));
#32009=CARTESIAN_POINT('Ctrl Pts',(1.81655087183054,-1.,-1.22921864890975));
#32010=CARTESIAN_POINT('Ctrl Pts',(1.81655087183054,1.,-1.22921864890975));
#32011=CARTESIAN_POINT('Ctrl Pts',(1.81817389920914,-1.,-1.23274224526804));
#32012=CARTESIAN_POINT('Ctrl Pts',(1.81817389920914,1.,-1.23274224526804));
#32013=CARTESIAN_POINT('Ctrl Pts',(1.81925017193531,-1.,-1.23509651170384));
#32014=CARTESIAN_POINT('Ctrl Pts',(1.81925017193531,1.,-1.23509651170384));
#32015=CARTESIAN_POINT('Ctrl Pts',(1.81978687191668,-1.,-1.23627494547115));
#32016=CARTESIAN_POINT('Ctrl Pts',(1.81978687191668,1.,-1.23627494547115));
#32017=CARTESIAN_POINT('',(1.5055822144029,1.,-0.892032620296855));
#32018=CARTESIAN_POINT('Ctrl Pts',(1.5055822144029,1.,-0.892032620296855));
#32019=CARTESIAN_POINT('Ctrl Pts',(1.50980486807181,1.,-0.894452006967538));
#32020=CARTESIAN_POINT('Ctrl Pts',(1.51805569591479,1.,-0.89918504749193));
#32021=CARTESIAN_POINT('Ctrl Pts',(1.52984849890434,1.,-0.905967409640499));
#32022=CARTESIAN_POINT('Ctrl Pts',(1.54440491152807,1.,-0.91437591904658));
#32023=CARTESIAN_POINT('Ctrl Pts',(1.56065988582509,1.,-0.923832188966322));
#32024=CARTESIAN_POINT('Ctrl Pts',(1.57499388385561,1.,-0.932246680128849));
#32025=CARTESIAN_POINT('Ctrl Pts',(1.58744937489796,1.,-0.939646377909319));
#32026=CARTESIAN_POINT('Ctrl Pts',(1.59810042045408,1.,-0.946078063325796));
#32027=CARTESIAN_POINT('Ctrl Pts',(1.60706069897794,1.,-0.951613284361248));
#32028=CARTESIAN_POINT('Ctrl Pts',(1.61449324337233,1.,-0.956354422921573));
#32029=CARTESIAN_POINT('Ctrl Pts',(1.62061638139929,1.,-0.960438326099958));
#32030=CARTESIAN_POINT('Ctrl Pts',(1.6257193066974,1.,-0.964046107037821));
#32031=CARTESIAN_POINT('Ctrl Pts',(1.63013849959083,1.,-0.967387853228041));
#32032=CARTESIAN_POINT('Ctrl Pts',(1.63420665729609,1.,-0.970669715996356));
#32033=CARTESIAN_POINT('Ctrl Pts',(1.63820952658157,1.,-0.974066058287501));
#32034=CARTESIAN_POINT('Ctrl Pts',(1.64233990826831,1.,-0.977689794120297));
#32035=CARTESIAN_POINT('Ctrl Pts',(1.64665139190834,1.,-0.981562530940574));
#32036=CARTESIAN_POINT('Ctrl Pts',(1.6511001661277,1.,-0.985642622921626));
#32037=CARTESIAN_POINT('Ctrl Pts',(1.65559044289746,1.,-0.98985562785445));
#32038=CARTESIAN_POINT('Ctrl Pts',(1.66001553809916,1.,-0.994121836661116));
#32039=CARTESIAN_POINT('Ctrl Pts',(1.66430758030304,1.,-0.998389654952317));
#32040=CARTESIAN_POINT('Ctrl Pts',(1.66846059277231,1.,-1.00265091003682));
#32041=CARTESIAN_POINT('Ctrl Pts',(1.67250335383248,1.,-1.00692206696387));
#32042=CARTESIAN_POINT('Ctrl Pts',(1.67648246776457,1.,-1.01123236493507));
#32043=CARTESIAN_POINT('Ctrl Pts',(1.6804428989482,1.,-1.01561026162787));
#32044=CARTESIAN_POINT('Ctrl Pts',(1.68440578021739,1.,-1.02006795074222));
#32045=CARTESIAN_POINT('Ctrl Pts',(1.68836910178475,1.,-1.02460180535272));
#32046=CARTESIAN_POINT('Ctrl Pts',(1.69231840863471,1.,-1.02919977579155));
#32047=CARTESIAN_POINT('Ctrl Pts',(1.69623414782769,1.,-1.03384646003587));
#32048=CARTESIAN_POINT('Ctrl Pts',(1.70010052930951,1.,-1.03852922490782));
#32049=CARTESIAN_POINT('Ctrl Pts',(1.70391338707969,1.,-1.04324363334546));
#32050=CARTESIAN_POINT('Ctrl Pts',(1.70767646263641,1.,-1.0479908540499));
#32051=CARTESIAN_POINT('Ctrl Pts',(1.71139783543986,1.,-1.05277517202854));
#32052=CARTESIAN_POINT('Ctrl Pts',(1.71508654427022,1.,-1.05760163192481));
#32053=CARTESIAN_POINT('Ctrl Pts',(1.71874858456908,1.,-1.0624732468065));
#32054=CARTESIAN_POINT('Ctrl Pts',(1.72238500928456,1.,-1.06738966975463));
#32055=CARTESIAN_POINT('Ctrl Pts',(1.72599406198489,1.,-1.07234866990252));
#32056=CARTESIAN_POINT('Ctrl Pts',(1.72957248977424,1.,-1.0773470373727));
#32057=CARTESIAN_POINT('Ctrl Pts',(1.73311705663407,1.,-1.08238162784749));
#32058=CARTESIAN_POINT('Ctrl Pts',(1.73662628326093,1.,-1.08745056285429));
#32059=CARTESIAN_POINT('Ctrl Pts',(1.74010053962252,1.,-1.09255329056496));
#32060=CARTESIAN_POINT('Ctrl Pts',(1.74354119236212,1.,-1.09768999241229));
#32061=CARTESIAN_POINT('Ctrl Pts',(1.74695004214924,1.,-1.10286118991144));
#32062=CARTESIAN_POINT('Ctrl Pts',(1.75032866075914,1.,-1.10806728183003));
#32063=CARTESIAN_POINT('Ctrl Pts',(1.75367772094617,1.,-1.11330807582542));
#32064=CARTESIAN_POINT('Ctrl Pts',(1.75699720772089,1.,-1.11858293216752));
#32065=CARTESIAN_POINT('Ctrl Pts',(1.76028671825084,1.,-1.12389096855078));
#32066=CARTESIAN_POINT('Ctrl Pts',(1.76354571966171,1.,-1.12923123555076));
#32067=CARTESIAN_POINT('Ctrl Pts',(1.76677384551883,1.,-1.13460291804635));
#32068=CARTESIAN_POINT('Ctrl Pts',(1.76997111386806,1.,-1.14000548337));
#32069=CARTESIAN_POINT('Ctrl Pts',(1.77313777896234,1.,-1.14543858226948));
#32070=CARTESIAN_POINT('Ctrl Pts',(1.77627422557034,1.,-1.15090197841531));
#32071=CARTESIAN_POINT('Ctrl Pts',(1.77938085564261,1.,-1.15639547194689));
#32072=CARTESIAN_POINT('Ctrl Pts',(1.78245795880949,1.,-1.16191881298458));
#32073=CARTESIAN_POINT('Ctrl Pts',(1.78550566040349,1.,-1.16747166312239));
#32074=CARTESIAN_POINT('Ctrl Pts',(1.78852398877523,1.,-1.17305363177265));
#32075=CARTESIAN_POINT('Ctrl Pts',(1.79151291552646,1.,-1.17866429440781));
#32076=CARTESIAN_POINT('Ctrl Pts',(1.79447240321572,1.,-1.18430321697471));
#32077=CARTESIAN_POINT('Ctrl Pts',(1.79740245923649,1.,-1.1899699793456));
#32078=CARTESIAN_POINT('Ctrl Pts',(1.80030314370121,1.,-1.19566418930405));
#32079=CARTESIAN_POINT('Ctrl Pts',(1.8031745483882,1.,-1.2013854893912));
#32080=CARTESIAN_POINT('Ctrl Pts',(1.80601678480772,1.,-1.20713356605519));
#32081=CARTESIAN_POINT('Ctrl Pts',(1.80882996916931,1.,-1.2129081570818));
#32082=CARTESIAN_POINT('Ctrl Pts',(1.81161420806172,1.,-1.2187090610323));
#32083=CARTESIAN_POINT('Ctrl Pts',(1.81436959209778,1.,-1.22453613304507));
#32084=CARTESIAN_POINT('Ctrl Pts',(1.81655087183054,1.,-1.22921864890975));
#32085=CARTESIAN_POINT('Ctrl Pts',(1.81817389920914,1.,-1.23274224526804));
#32086=CARTESIAN_POINT('Ctrl Pts',(1.81925017193531,1.,-1.23509651170384));
#32087=CARTESIAN_POINT('Ctrl Pts',(1.81978687191668,1.,-1.23627494547115));
#32088=CARTESIAN_POINT('',(1.5055822144029,0.,-0.892032620296855));
#32089=CARTESIAN_POINT('Origin',(0.,0.,0.));
#32090=CARTESIAN_POINT('',(1.60662857109684,1.,-0.693717979106306));
#32091=CARTESIAN_POINT('Origin',(0.,1.,0.));
#32092=CARTESIAN_POINT('',(1.60662857109684,0.,-0.693717979106308));
#32093=CARTESIAN_POINT('Ctrl Pts',(2.0698113262342,-1.,-0.745574324794401));
#32094=CARTESIAN_POINT('Ctrl Pts',(2.0698113262342,1.,-0.745574324794401));
#32095=CARTESIAN_POINT('Ctrl Pts',(2.06854248895728,-1.,-0.745832791378367));
#32096=CARTESIAN_POINT('Ctrl Pts',(2.06854248895728,1.,-0.745832791378367));
#32097=CARTESIAN_POINT('Ctrl Pts',(2.06600523016815,-1.,-0.746345871544201));
#32098=CARTESIAN_POINT('Ctrl Pts',(2.06600523016815,1.,-0.746345871544201));
#32099=CARTESIAN_POINT('Ctrl Pts',(2.06220058927826,-1.,-0.74710393278792));
#32100=CARTESIAN_POINT('Ctrl Pts',(2.06220058927826,1.,-0.74710393278792));
#32101=CARTESIAN_POINT('Ctrl Pts',(2.05713023031006,-1.,-0.748091554183803));
#32102=CARTESIAN_POINT('Ctrl Pts',(2.05713023031006,1.,-0.748091554183803));
#32103=CARTESIAN_POINT('Ctrl Pts',(2.05079645592154,-1.,-0.749287468665046));
#32104=CARTESIAN_POINT('Ctrl Pts',(2.05079645592154,1.,-0.749287468665046));
#32105=CARTESIAN_POINT('Ctrl Pts',(2.04446689147979,-1.,-0.750444657875576));
#32106=CARTESIAN_POINT('Ctrl Pts',(2.04446689147979,1.,-0.750444657875576));
#32107=CARTESIAN_POINT('Ctrl Pts',(2.03814160092099,-1.,-0.751562963361115));
#32108=CARTESIAN_POINT('Ctrl Pts',(2.03814160092099,1.,-0.751562963361115));
#32109=CARTESIAN_POINT('Ctrl Pts',(2.03182068456221,-1.,-0.752642180487211));
#32110=CARTESIAN_POINT('Ctrl Pts',(2.03182068456221,1.,-0.752642180487211));
#32111=CARTESIAN_POINT('Ctrl Pts',(2.02550428623313,-1.,-0.753682061112768));
#32112=CARTESIAN_POINT('Ctrl Pts',(2.02550428623313,1.,-0.753682061112768));
#32113=CARTESIAN_POINT('Ctrl Pts',(2.01919259405809,-1.,-0.754682330722816));
#32114=CARTESIAN_POINT('Ctrl Pts',(2.01919259405809,1.,-0.754682330722816));
#32115=CARTESIAN_POINT('Ctrl Pts',(2.01288584328084,-1.,-0.755642704957865));
#32116=CARTESIAN_POINT('Ctrl Pts',(2.01288584328084,1.,-0.755642704957865));
#32117=CARTESIAN_POINT('Ctrl Pts',(2.0065843158773,-1.,-0.756562904646671));
#32118=CARTESIAN_POINT('Ctrl Pts',(2.0065843158773,1.,-0.756562904646671));
#32119=CARTESIAN_POINT('Ctrl Pts',(2.00028834739178,-1.,-0.757442676862724));
#32120=CARTESIAN_POINT('Ctrl Pts',(2.00028834739178,1.,-0.757442676862724));
#32121=CARTESIAN_POINT('Ctrl Pts',(1.99399831098817,-1.,-0.758281796766761));
#32122=CARTESIAN_POINT('Ctrl Pts',(1.99399831098817,1.,-0.758281796766761));
#32123=CARTESIAN_POINT('Ctrl Pts',(1.98771456680874,-1.,-0.759080037802488));
#32124=CARTESIAN_POINT('Ctrl Pts',(1.98771456680874,1.,-0.759080037802488));
#32125=CARTESIAN_POINT('Ctrl Pts',(1.98143741418172,-1.,-0.75983714745219));
#32126=CARTESIAN_POINT('Ctrl Pts',(1.98143741418172,1.,-0.75983714745219));
#32127=CARTESIAN_POINT('Ctrl Pts',(1.97516705321494,-1.,-0.760552825409757));
#32128=CARTESIAN_POINT('Ctrl Pts',(1.97516705321494,1.,-0.760552825409757));
#32129=CARTESIAN_POINT('Ctrl Pts',(1.96890351582499,-1.,-0.761226690483821));
#32130=CARTESIAN_POINT('Ctrl Pts',(1.96890351582499,1.,-0.761226690483821));
#32131=CARTESIAN_POINT('Ctrl Pts',(1.96264672744186,-1.,-0.761858300014424));
#32132=CARTESIAN_POINT('Ctrl Pts',(1.96264672744186,1.,-0.761858300014424));
#32133=CARTESIAN_POINT('Ctrl Pts',(1.95639665309869,-1.,-0.762447203806179));
#32134=CARTESIAN_POINT('Ctrl Pts',(1.95639665309869,1.,-0.762447203806179));
#32135=CARTESIAN_POINT('Ctrl Pts',(1.95015342590024,-1.,-0.762992990878769));
#32136=CARTESIAN_POINT('Ctrl Pts',(1.95015342590024,1.,-0.762992990878769));
#32137=CARTESIAN_POINT('Ctrl Pts',(1.9439174661764,-1.,-0.763495333538629));
#32138=CARTESIAN_POINT('Ctrl Pts',(1.9439174661764,1.,-0.763495333538629));
#32139=CARTESIAN_POINT('Ctrl Pts',(1.93768964875886,-1.,-0.763954049121459));
#32140=CARTESIAN_POINT('Ctrl Pts',(1.93768964875886,1.,-0.763954049121459));
#32141=CARTESIAN_POINT('Ctrl Pts',(1.93147105496382,-1.,-0.764369010673941));
#32142=CARTESIAN_POINT('Ctrl Pts',(1.93147105496382,1.,-0.764369010673941));
#32143=CARTESIAN_POINT('Ctrl Pts',(1.92526263537048,-1.,-0.764740025488212));
#32144=CARTESIAN_POINT('Ctrl Pts',(1.92526263537048,1.,-0.764740025488212));
#32145=CARTESIAN_POINT('Ctrl Pts',(1.91906491634196,-1.,-0.765066729667089));
#32146=CARTESIAN_POINT('Ctrl Pts',(1.91906491634196,1.,-0.765066729667089));
#32147=CARTESIAN_POINT('Ctrl Pts',(1.91287765805169,-1.,-0.765348465884722));
#32148=CARTESIAN_POINT('Ctrl Pts',(1.91287765805169,1.,-0.765348465884722));
#32149=CARTESIAN_POINT('Ctrl Pts',(1.90669961402356,-1.,-0.765584196937919));
#32150=CARTESIAN_POINT('Ctrl Pts',(1.90669961402356,1.,-0.765584196937919));
#32151=CARTESIAN_POINT('Ctrl Pts',(1.90052930393596,-1.,-0.765772772593386));
#32152=CARTESIAN_POINT('Ctrl Pts',(1.90052930393596,1.,-0.765772772593386));
#32153=CARTESIAN_POINT('Ctrl Pts',(1.89436577771388,-1.,-0.765913193856978));
#32154=CARTESIAN_POINT('Ctrl Pts',(1.89436577771388,1.,-0.765913193856978));
#32155=CARTESIAN_POINT('Ctrl Pts',(1.88820926433409,-1.,-0.766004837062091));
#32156=CARTESIAN_POINT('Ctrl Pts',(1.88820926433409,1.,-0.766004837062091));
#32157=CARTESIAN_POINT('Ctrl Pts',(1.88206215302561,-1.,-0.766047794851865));
#32158=CARTESIAN_POINT('Ctrl Pts',(1.88206215302561,1.,-0.766047794851865));
#32159=CARTESIAN_POINT('Ctrl Pts',(1.87592888967883,-1.,-0.766042837036744));
#32160=CARTESIAN_POINT('Ctrl Pts',(1.87592888967883,1.,-0.766042837036744));
#32161=CARTESIAN_POINT('Ctrl Pts',(1.86981398314341,-1.,-0.765990708546091));
#32162=CARTESIAN_POINT('Ctrl Pts',(1.86981398314341,1.,-0.765990708546091));
#32163=CARTESIAN_POINT('Ctrl Pts',(1.86372027063312,-1.,-0.765891519092547));
#32164=CARTESIAN_POINT('Ctrl Pts',(1.86372027063312,1.,-0.765891519092547));
#32165=CARTESIAN_POINT('Ctrl Pts',(1.85764741390394,-1.,-0.765744212909319));
#32166=CARTESIAN_POINT('Ctrl Pts',(1.85764741390394,1.,-0.765744212909319));
#32167=CARTESIAN_POINT('Ctrl Pts',(1.85158945130063,-1.,-0.765545710619063));
#32168=CARTESIAN_POINT('Ctrl Pts',(1.85158945130063,1.,-0.765545710619063));
#32169=CARTESIAN_POINT('Ctrl Pts',(1.84553698875924,-1.,-0.765291664862029));
#32170=CARTESIAN_POINT('Ctrl Pts',(1.84553698875924,1.,-0.765291664862029));
#32171=CARTESIAN_POINT('Ctrl Pts',(1.83948181064835,-1.,-0.764978057881738));
#32172=CARTESIAN_POINT('Ctrl Pts',(1.83948181064835,1.,-0.764978057881738));
#32173=CARTESIAN_POINT('Ctrl Pts',(1.83342077227142,-1.,-0.764602549687853));
#32174=CARTESIAN_POINT('Ctrl Pts',(1.83342077227142,1.,-0.764602549687853));
#32175=CARTESIAN_POINT('Ctrl Pts',(1.82735991200065,-1.,-0.764165902605995));
#32176=CARTESIAN_POINT('Ctrl Pts',(1.82735991200065,1.,-0.764165902605995));
#32177=CARTESIAN_POINT('Ctrl Pts',(1.82131873145266,-1.,-0.763673465462727));
#32178=CARTESIAN_POINT('Ctrl Pts',(1.82131873145266,1.,-0.763673465462727));
#32179=CARTESIAN_POINT('Ctrl Pts',(1.8153211840553,-1.,-0.763132003836634));
#32180=CARTESIAN_POINT('Ctrl Pts',(1.8153211840553,1.,-0.763132003836634));
#32181=CARTESIAN_POINT('Ctrl Pts',(1.80938551463965,-1.,-0.762546129463938));
#32182=CARTESIAN_POINT('Ctrl Pts',(1.80938551463965,1.,-0.762546129463938));
#32183=CARTESIAN_POINT('Ctrl Pts',(1.80351583877342,-1.,-0.761915336443547));
#32184=CARTESIAN_POINT('Ctrl Pts',(1.80351583877342,1.,-0.761915336443547));
#32185=CARTESIAN_POINT('Ctrl Pts',(1.79768986997783,-1.,-0.761229695230558));
#32186=CARTESIAN_POINT('Ctrl Pts',(1.79768986997783,1.,-0.761229695230558));
#32187=CARTESIAN_POINT('Ctrl Pts',(1.7918581561088,-1.,-0.760469555880749));
#32188=CARTESIAN_POINT('Ctrl Pts',(1.7918581561088,1.,-0.760469555880749));
#32189=CARTESIAN_POINT('Ctrl Pts',(1.78596964884604,-1.,-0.75961440111019));
#32190=CARTESIAN_POINT('Ctrl Pts',(1.78596964884604,1.,-0.75961440111019));
#32191=CARTESIAN_POINT('Ctrl Pts',(1.77999411220945,-1.,-0.758650626677519));
#32192=CARTESIAN_POINT('Ctrl Pts',(1.77999411220945,1.,-0.758650626677519));
#32193=CARTESIAN_POINT('Ctrl Pts',(1.77394167108292,-1.,-0.757578264077029));
#32194=CARTESIAN_POINT('Ctrl Pts',(1.77394167108292,1.,-0.757578264077029));
#32195=CARTESIAN_POINT('Ctrl Pts',(1.76789396002998,-1.,-0.75642189602781));
#32196=CARTESIAN_POINT('Ctrl Pts',(1.76789396002998,1.,-0.75642189602781));
#32197=CARTESIAN_POINT('Ctrl Pts',(1.76197817240128,-1.,-0.755220979974462));
#32198=CARTESIAN_POINT('Ctrl Pts',(1.76197817240128,1.,-0.755220979974462));
#32199=CARTESIAN_POINT('Ctrl Pts',(1.75631083600019,-1.,-0.754009254027829));
#32200=CARTESIAN_POINT('Ctrl Pts',(1.75631083600019,1.,-0.754009254027829));
#32201=CARTESIAN_POINT('Ctrl Pts',(1.75095139468794,-1.,-0.752797683531314));
#32202=CARTESIAN_POINT('Ctrl Pts',(1.75095139468794,1.,-0.752797683531314));
#32203=CARTESIAN_POINT('Ctrl Pts',(1.74585086852502,-1.,-0.751555614164483));
#32204=CARTESIAN_POINT('Ctrl Pts',(1.74585086852502,1.,-0.751555614164483));
#32205=CARTESIAN_POINT('Ctrl Pts',(1.74080458267114,-1.,-0.75019343598125));
#32206=CARTESIAN_POINT('Ctrl Pts',(1.74080458267114,1.,-0.75019343598125));
#32207=CARTESIAN_POINT('Ctrl Pts',(1.7355035168033,-1.,-0.74858246295687));
#32208=CARTESIAN_POINT('Ctrl Pts',(1.7355035168033,1.,-0.74858246295687));
#32209=CARTESIAN_POINT('Ctrl Pts',(1.72958533647714,-1.,-0.746574710097752));
#32210=CARTESIAN_POINT('Ctrl Pts',(1.72958533647714,1.,-0.746574710097752));
#32211=CARTESIAN_POINT('Ctrl Pts',(1.72268229916769,-1.,-0.744021445433094));
#32212=CARTESIAN_POINT('Ctrl Pts',(1.72268229916769,1.,-0.744021445433094));
#32213=CARTESIAN_POINT('Ctrl Pts',(1.71447789751001,-1.,-0.74079516202821));
#32214=CARTESIAN_POINT('Ctrl Pts',(1.71447789751001,1.,-0.74079516202821));
#32215=CARTESIAN_POINT('Ctrl Pts',(1.70473309004249,-1.,-0.736799665716932));
#32216=CARTESIAN_POINT('Ctrl Pts',(1.70473309004249,1.,-0.736799665716932));
#32217=CARTESIAN_POINT('Ctrl Pts',(1.69326921972915,-1.,-0.731963238685357));
#32218=CARTESIAN_POINT('Ctrl Pts',(1.69326921972915,1.,-0.731963238685357));
#32219=CARTESIAN_POINT('Ctrl Pts',(1.67996158451922,-1.,-0.726235967982445));
#32220=CARTESIAN_POINT('Ctrl Pts',(1.67996158451922,1.,-0.726235967982445));
#32221=CARTESIAN_POINT('Ctrl Pts',(1.66472880551777,-1.,-0.71958543378795));
#32222=CARTESIAN_POINT('Ctrl Pts',(1.66472880551777,1.,-0.71958543378795));
#32223=CARTESIAN_POINT('Ctrl Pts',(1.64752408828442,-1.,-0.711993139340448));
#32224=CARTESIAN_POINT('Ctrl Pts',(1.64752408828442,1.,-0.711993139340448));
#32225=CARTESIAN_POINT('Ctrl Pts',(1.6321654166204,-1.,-0.705159151977294));
#32226=CARTESIAN_POINT('Ctrl Pts',(1.6321654166204,1.,-0.705159151977294));
#32227=CARTESIAN_POINT('Ctrl Pts',(1.61974673471117,-1.,-0.699605146398837));
#32228=CARTESIAN_POINT('Ctrl Pts',(1.61974673471117,1.,-0.699605146398837));
#32229=CARTESIAN_POINT('Ctrl Pts',(1.61106790957619,-1.,-0.69571209787897));
#32230=CARTESIAN_POINT('Ctrl Pts',(1.61106790957619,1.,-0.69571209787897));
#32231=CARTESIAN_POINT('Ctrl Pts',(1.60662857109684,-1.,-0.693717979106306));
#32232=CARTESIAN_POINT('Ctrl Pts',(1.60662857109684,1.,-0.693717979106306));
#32233=CARTESIAN_POINT('',(2.0698113262342,1.,-0.745574324794401));
#32234=CARTESIAN_POINT('Ctrl Pts',(2.0698113262342,1.,-0.745574324794401));
#32235=CARTESIAN_POINT('Ctrl Pts',(2.06854248895728,1.,-0.745832791378367));
#32236=CARTESIAN_POINT('Ctrl Pts',(2.06600523016815,1.,-0.746345871544201));
#32237=CARTESIAN_POINT('Ctrl Pts',(2.06220058927826,1.,-0.74710393278792));
#32238=CARTESIAN_POINT('Ctrl Pts',(2.05713023031006,1.,-0.748091554183803));
#32239=CARTESIAN_POINT('Ctrl Pts',(2.05079645592154,1.,-0.749287468665046));
#32240=CARTESIAN_POINT('Ctrl Pts',(2.04446689147979,1.,-0.750444657875576));
#32241=CARTESIAN_POINT('Ctrl Pts',(2.03814160092099,1.,-0.751562963361115));
#32242=CARTESIAN_POINT('Ctrl Pts',(2.03182068456221,1.,-0.752642180487211));
#32243=CARTESIAN_POINT('Ctrl Pts',(2.02550428623313,1.,-0.753682061112768));
#32244=CARTESIAN_POINT('Ctrl Pts',(2.01919259405809,1.,-0.754682330722816));
#32245=CARTESIAN_POINT('Ctrl Pts',(2.01288584328084,1.,-0.755642704957865));
#32246=CARTESIAN_POINT('Ctrl Pts',(2.0065843158773,1.,-0.756562904646671));
#32247=CARTESIAN_POINT('Ctrl Pts',(2.00028834739178,1.,-0.757442676862724));
#32248=CARTESIAN_POINT('Ctrl Pts',(1.99399831098817,1.,-0.758281796766761));
#32249=CARTESIAN_POINT('Ctrl Pts',(1.98771456680874,1.,-0.759080037802488));
#32250=CARTESIAN_POINT('Ctrl Pts',(1.98143741418172,1.,-0.75983714745219));
#32251=CARTESIAN_POINT('Ctrl Pts',(1.97516705321494,1.,-0.760552825409757));
#32252=CARTESIAN_POINT('Ctrl Pts',(1.96890351582499,1.,-0.761226690483821));
#32253=CARTESIAN_POINT('Ctrl Pts',(1.96264672744186,1.,-0.761858300014424));
#32254=CARTESIAN_POINT('Ctrl Pts',(1.95639665309869,1.,-0.762447203806179));
#32255=CARTESIAN_POINT('Ctrl Pts',(1.95015342590024,1.,-0.762992990878769));
#32256=CARTESIAN_POINT('Ctrl Pts',(1.9439174661764,1.,-0.763495333538629));
#32257=CARTESIAN_POINT('Ctrl Pts',(1.93768964875886,1.,-0.763954049121459));
#32258=CARTESIAN_POINT('Ctrl Pts',(1.93147105496382,1.,-0.764369010673941));
#32259=CARTESIAN_POINT('Ctrl Pts',(1.92526263537048,1.,-0.764740025488212));
#32260=CARTESIAN_POINT('Ctrl Pts',(1.91906491634196,1.,-0.765066729667089));
#32261=CARTESIAN_POINT('Ctrl Pts',(1.91287765805169,1.,-0.765348465884722));
#32262=CARTESIAN_POINT('Ctrl Pts',(1.90669961402356,1.,-0.765584196937919));
#32263=CARTESIAN_POINT('Ctrl Pts',(1.90052930393596,1.,-0.765772772593386));
#32264=CARTESIAN_POINT('Ctrl Pts',(1.89436577771388,1.,-0.765913193856978));
#32265=CARTESIAN_POINT('Ctrl Pts',(1.88820926433409,1.,-0.766004837062091));
#32266=CARTESIAN_POINT('Ctrl Pts',(1.88206215302561,1.,-0.766047794851865));
#32267=CARTESIAN_POINT('Ctrl Pts',(1.87592888967883,1.,-0.766042837036744));
#32268=CARTESIAN_POINT('Ctrl Pts',(1.86981398314341,1.,-0.765990708546091));
#32269=CARTESIAN_POINT('Ctrl Pts',(1.86372027063312,1.,-0.765891519092547));
#32270=CARTESIAN_POINT('Ctrl Pts',(1.85764741390394,1.,-0.765744212909319));
#32271=CARTESIAN_POINT('Ctrl Pts',(1.85158945130063,1.,-0.765545710619063));
#32272=CARTESIAN_POINT('Ctrl Pts',(1.84553698875924,1.,-0.765291664862029));
#32273=CARTESIAN_POINT('Ctrl Pts',(1.83948181064835,1.,-0.764978057881738));
#32274=CARTESIAN_POINT('Ctrl Pts',(1.83342077227142,1.,-0.764602549687853));
#32275=CARTESIAN_POINT('Ctrl Pts',(1.82735991200065,1.,-0.764165902605995));
#32276=CARTESIAN_POINT('Ctrl Pts',(1.82131873145266,1.,-0.763673465462727));
#32277=CARTESIAN_POINT('Ctrl Pts',(1.8153211840553,1.,-0.763132003836634));
#32278=CARTESIAN_POINT('Ctrl Pts',(1.80938551463965,1.,-0.762546129463938));
#32279=CARTESIAN_POINT('Ctrl Pts',(1.80351583877342,1.,-0.761915336443547));
#32280=CARTESIAN_POINT('Ctrl Pts',(1.79768986997783,1.,-0.761229695230558));
#32281=CARTESIAN_POINT('Ctrl Pts',(1.7918581561088,1.,-0.760469555880749));
#32282=CARTESIAN_POINT('Ctrl Pts',(1.78596964884604,1.,-0.75961440111019));
#32283=CARTESIAN_POINT('Ctrl Pts',(1.77999411220945,1.,-0.758650626677519));
#32284=CARTESIAN_POINT('Ctrl Pts',(1.77394167108292,1.,-0.757578264077029));
#32285=CARTESIAN_POINT('Ctrl Pts',(1.76789396002998,1.,-0.75642189602781));
#32286=CARTESIAN_POINT('Ctrl Pts',(1.76197817240128,1.,-0.755220979974462));
#32287=CARTESIAN_POINT('Ctrl Pts',(1.75631083600019,1.,-0.754009254027829));
#32288=CARTESIAN_POINT('Ctrl Pts',(1.75095139468794,1.,-0.752797683531314));
#32289=CARTESIAN_POINT('Ctrl Pts',(1.74585086852502,1.,-0.751555614164483));
#32290=CARTESIAN_POINT('Ctrl Pts',(1.74080458267114,1.,-0.75019343598125));
#32291=CARTESIAN_POINT('Ctrl Pts',(1.7355035168033,1.,-0.74858246295687));
#32292=CARTESIAN_POINT('Ctrl Pts',(1.72958533647714,1.,-0.746574710097752));
#32293=CARTESIAN_POINT('Ctrl Pts',(1.72268229916769,1.,-0.744021445433094));
#32294=CARTESIAN_POINT('Ctrl Pts',(1.71447789751001,1.,-0.74079516202821));
#32295=CARTESIAN_POINT('Ctrl Pts',(1.70473309004249,1.,-0.736799665716932));
#32296=CARTESIAN_POINT('Ctrl Pts',(1.69326921972915,1.,-0.731963238685357));
#32297=CARTESIAN_POINT('Ctrl Pts',(1.67996158451922,1.,-0.726235967982445));
#32298=CARTESIAN_POINT('Ctrl Pts',(1.66472880551777,1.,-0.71958543378795));
#32299=CARTESIAN_POINT('Ctrl Pts',(1.64752408828442,1.,-0.711993139340448));
#32300=CARTESIAN_POINT('Ctrl Pts',(1.6321654166204,1.,-0.705159151977294));
#32301=CARTESIAN_POINT('Ctrl Pts',(1.61974673471117,1.,-0.699605146398837));
#32302=CARTESIAN_POINT('Ctrl Pts',(1.61106790957619,1.,-0.69571209787897));
#32303=CARTESIAN_POINT('Ctrl Pts',(1.60662857109684,1.,-0.693717979106306));
#32304=CARTESIAN_POINT('',(2.0698113262342,0.,-0.745574324794401));
#32305=CARTESIAN_POINT('Origin',(2.11275013067528,0.,-0.61342227326009));
#32306=CARTESIAN_POINT('',(2.11275013067528,1.,-0.61342227326009));
#32307=CARTESIAN_POINT('',(2.0698113262342,1.,-0.745574324794401));
#32308=CARTESIAN_POINT('',(2.11275013067528,0.,-0.61342227326009));
#32309=CARTESIAN_POINT('Ctrl Pts',(1.7075470150345,-1.,-0.383122945602004));
#32310=CARTESIAN_POINT('Ctrl Pts',(1.7075470150345,1.,-0.383122945602004));
#32311=CARTESIAN_POINT('Ctrl Pts',(1.71231062891958,-1.,-0.384119047315542));
#32312=CARTESIAN_POINT('Ctrl Pts',(1.71231062891958,1.,-0.384119047315542));
#32313=CARTESIAN_POINT('Ctrl Pts',(1.72162022246158,-1.,-0.38607079032701));
#32314=CARTESIAN_POINT('Ctrl Pts',(1.72162022246158,1.,-0.38607079032701));
#32315=CARTESIAN_POINT('Ctrl Pts',(1.7349317097561,-1.,-0.388877023509192));
#32316=CARTESIAN_POINT('Ctrl Pts',(1.7349317097561,1.,-0.388877023509192));
#32317=CARTESIAN_POINT('Ctrl Pts',(1.75137405313962,-1.,-0.392375812294307));
#32318=CARTESIAN_POINT('Ctrl Pts',(1.75137405313962,1.,-0.392375812294307));
#32319=CARTESIAN_POINT('Ctrl Pts',(1.7697556004756,-1.,-0.39634619612042));
#32320=CARTESIAN_POINT('Ctrl Pts',(1.7697556004756,1.,-0.39634619612042));
#32321=CARTESIAN_POINT('Ctrl Pts',(1.78598826347533,-1.,-0.399919403783081));
#32322=CARTESIAN_POINT('Ctrl Pts',(1.78598826347533,1.,-0.399919403783081));
#32323=CARTESIAN_POINT('Ctrl Pts',(1.80012077176221,-1.,-0.403107976170441));
#32324=CARTESIAN_POINT('Ctrl Pts',(1.80012077176221,1.,-0.403107976170441));
#32325=CARTESIAN_POINT('Ctrl Pts',(1.81223801813988,-1.,-0.405933518411838));
#32326=CARTESIAN_POINT('Ctrl Pts',(1.81223801813988,1.,-0.405933518411838));
#32327=CARTESIAN_POINT('Ctrl Pts',(1.8224702267854,-1.,-0.408428948108534));
#32328=CARTESIAN_POINT('Ctrl Pts',(1.8224702267854,1.,-0.408428948108534));
#32329=CARTESIAN_POINT('Ctrl Pts',(1.83100408895216,-1.,-0.410641256301675));
#32330=CARTESIAN_POINT('Ctrl Pts',(1.83100408895216,1.,-0.410641256301675));
#32331=CARTESIAN_POINT('Ctrl Pts',(1.83808953475839,-1.,-0.412633125322162));
#32332=CARTESIAN_POINT('Ctrl Pts',(1.83808953475839,1.,-0.412633125322162));
#32333=CARTESIAN_POINT('Ctrl Pts',(1.8440575707371,-1.,-0.41448743825434));
#32334=CARTESIAN_POINT('Ctrl Pts',(1.8440575707371,1.,-0.41448743825434));
#32335=CARTESIAN_POINT('Ctrl Pts',(1.84929312929882,-1.,-0.416300022038864));
#32336=CARTESIAN_POINT('Ctrl Pts',(1.84929312929882,1.,-0.416300022038864));
#32337=CARTESIAN_POINT('Ctrl Pts',(1.85417632856234,-1.,-0.418164129143534));
#32338=CARTESIAN_POINT('Ctrl Pts',(1.85417632856234,1.,-0.418164129143534));
#32339=CARTESIAN_POINT('Ctrl Pts',(1.85903281096686,-1.,-0.42015728797562));
#32340=CARTESIAN_POINT('Ctrl Pts',(1.85903281096686,1.,-0.42015728797562));
#32341=CARTESIAN_POINT('Ctrl Pts',(1.86408083334028,-1.,-0.422327307418275));
#32342=CARTESIAN_POINT('Ctrl Pts',(1.86408083334028,1.,-0.422327307418275));
#32343=CARTESIAN_POINT('Ctrl Pts',(1.86937803944323,-1.,-0.424678177291359));
#32344=CARTESIAN_POINT('Ctrl Pts',(1.86937803944323,1.,-0.424678177291359));
#32345=CARTESIAN_POINT('Ctrl Pts',(1.87486989291484,-1.,-0.427183828519102));
#32346=CARTESIAN_POINT('Ctrl Pts',(1.87486989291484,1.,-0.427183828519102));
#32347=CARTESIAN_POINT('Ctrl Pts',(1.88044229001832,-1.,-0.429803062482345));
#32348=CARTESIAN_POINT('Ctrl Pts',(1.88044229001832,1.,-0.429803062482345));
#32349=CARTESIAN_POINT('Ctrl Pts',(1.88596913666793,-1.,-0.432493038548748));
#32350=CARTESIAN_POINT('Ctrl Pts',(1.88596913666793,1.,-0.432493038548748));
#32351=CARTESIAN_POINT('Ctrl Pts',(1.89136993975504,-1.,-0.435225660963383));
#32352=CARTESIAN_POINT('Ctrl Pts',(1.89136993975504,1.,-0.435225660963383));
#32353=CARTESIAN_POINT('Ctrl Pts',(1.89663648956466,-1.,-0.437995003948244));
#32354=CARTESIAN_POINT('Ctrl Pts',(1.89663648956466,1.,-0.437995003948244));
#32355=CARTESIAN_POINT('Ctrl Pts',(1.90180124389086,-1.,-0.440807833704038));
#32356=CARTESIAN_POINT('Ctrl Pts',(1.90180124389086,1.,-0.440807833704038));
#32357=CARTESIAN_POINT('Ctrl Pts',(1.90691756144898,-1.,-0.443677556849151));
#32358=CARTESIAN_POINT('Ctrl Pts',(1.90691756144898,1.,-0.443677556849151));
#32359=CARTESIAN_POINT('Ctrl Pts',(1.9120369998112,-1.,-0.446617343485711));
#32360=CARTESIAN_POINT('Ctrl Pts',(1.9120369998112,1.,-0.446617343485711));
#32361=CARTESIAN_POINT('Ctrl Pts',(1.91718342555755,-1.,-0.449632260106662));
#32362=CARTESIAN_POINT('Ctrl Pts',(1.91718342555755,1.,-0.449632260106662));
#32363=CARTESIAN_POINT('Ctrl Pts',(1.92235380648502,-1.,-0.452719478359433));
#32364=CARTESIAN_POINT('Ctrl Pts',(1.92235380648502,1.,-0.452719478359433));
#32365=CARTESIAN_POINT('Ctrl Pts',(1.92753067150476,-1.,-0.455872005174371));
#32366=CARTESIAN_POINT('Ctrl Pts',(1.92753067150476,1.,-0.455872005174371));
#32367=CARTESIAN_POINT('Ctrl Pts',(1.93269066517934,-1.,-0.459081234547926));
#32368=CARTESIAN_POINT('Ctrl Pts',(1.93269066517934,1.,-0.459081234547926));
#32369=CARTESIAN_POINT('Ctrl Pts',(1.93781486640821,-1.,-0.462340031009057));
#32370=CARTESIAN_POINT('Ctrl Pts',(1.93781486640821,1.,-0.462340031009057));
#32371=CARTESIAN_POINT('Ctrl Pts',(1.9428979419619,-1.,-0.46564546202603));
#32372=CARTESIAN_POINT('Ctrl Pts',(1.9428979419619,1.,-0.46564546202603));
#32373=CARTESIAN_POINT('Ctrl Pts',(1.94794381136514,-1.,-0.468997482913135));
#32374=CARTESIAN_POINT('Ctrl Pts',(1.94794381136514,1.,-0.468997482913135));
#32375=CARTESIAN_POINT('Ctrl Pts',(1.95296148278133,-1.,-0.472397672264072));
#32376=CARTESIAN_POINT('Ctrl Pts',(1.95296148278133,1.,-0.472397672264072));
#32377=CARTESIAN_POINT('Ctrl Pts',(1.95796111148177,-1.,-0.475848034683176));
#32378=CARTESIAN_POINT('Ctrl Pts',(1.95796111148177,1.,-0.475848034683176));
#32379=CARTESIAN_POINT('Ctrl Pts',(1.96294933055943,-1.,-0.479349583074855));
#32380=CARTESIAN_POINT('Ctrl Pts',(1.96294933055943,1.,-0.479349583074855));
#32381=CARTESIAN_POINT('Ctrl Pts',(1.96792703422362,-1.,-0.482901662120691));
#32382=CARTESIAN_POINT('Ctrl Pts',(1.96792703422362,1.,-0.482901662120691));
#32383=CARTESIAN_POINT('Ctrl Pts',(1.97289186263272,-1.,-0.486502692907659));
#32384=CARTESIAN_POINT('Ctrl Pts',(1.97289186263272,1.,-0.486502692907659));
#32385=CARTESIAN_POINT('Ctrl Pts',(1.97783973019229,-1.,-0.490150627860953));
#32386=CARTESIAN_POINT('Ctrl Pts',(1.97783973019229,1.,-0.490150627860953));
#32387=CARTESIAN_POINT('Ctrl Pts',(1.98276658761821,-1.,-0.493843476541495));
#32388=CARTESIAN_POINT('Ctrl Pts',(1.98276658761821,1.,-0.493843476541495));
#32389=CARTESIAN_POINT('Ctrl Pts',(1.98767044752932,-1.,-0.497579909545574));
#32390=CARTESIAN_POINT('Ctrl Pts',(1.98767044752932,1.,-0.497579909545574));
#32391=CARTESIAN_POINT('Ctrl Pts',(1.99255149126155,-1.,-0.501359287727146));
#32392=CARTESIAN_POINT('Ctrl Pts',(1.99255149126155,1.,-0.501359287727146));
#32393=CARTESIAN_POINT('Ctrl Pts',(1.99741107463572,-1.,-0.505181361323026));
#32394=CARTESIAN_POINT('Ctrl Pts',(1.99741107463572,1.,-0.505181361323026));
#32395=CARTESIAN_POINT('Ctrl Pts',(2.00225107134734,-1.,-0.509046069886157));
#32396=CARTESIAN_POINT('Ctrl Pts',(2.00225107134734,1.,-0.509046069886157));
#32397=CARTESIAN_POINT('Ctrl Pts',(2.00707309946949,-1.,-0.512953306961793));
#32398=CARTESIAN_POINT('Ctrl Pts',(2.00707309946949,1.,-0.512953306961793));
#32399=CARTESIAN_POINT('Ctrl Pts',(2.01187773939242,-1.,-0.516902681728687));
#32400=CARTESIAN_POINT('Ctrl Pts',(2.01187773939242,1.,-0.516902681728687));
#32401=CARTESIAN_POINT('Ctrl Pts',(2.01666477917286,-1.,-0.520893590399371));
#32402=CARTESIAN_POINT('Ctrl Pts',(2.01666477917286,1.,-0.520893590399371));
#32403=CARTESIAN_POINT('Ctrl Pts',(2.02143356304698,-1.,-0.524925318333476));
#32404=CARTESIAN_POINT('Ctrl Pts',(2.02143356304698,1.,-0.524925318333476));
#32405=CARTESIAN_POINT('Ctrl Pts',(2.0261832908329,-1.,-0.528997127241914));
#32406=CARTESIAN_POINT('Ctrl Pts',(2.0261832908329,1.,-0.528997127241914));
#32407=CARTESIAN_POINT('Ctrl Pts',(2.03091336214426,-1.,-0.533108355132977));
#32408=CARTESIAN_POINT('Ctrl Pts',(2.03091336214426,1.,-0.533108355132977));
#32409=CARTESIAN_POINT('Ctrl Pts',(2.03562362954037,-1.,-0.537258489833262));
#32410=CARTESIAN_POINT('Ctrl Pts',(2.03562362954037,1.,-0.537258489833262));
#32411=CARTESIAN_POINT('Ctrl Pts',(2.04031422690527,-1.,-0.541447120615659));
#32412=CARTESIAN_POINT('Ctrl Pts',(2.04031422690527,1.,-0.541447120615659));
#32413=CARTESIAN_POINT('Ctrl Pts',(2.04498544714588,-1.,-0.54567390381743));
#32414=CARTESIAN_POINT('Ctrl Pts',(2.04498544714588,1.,-0.54567390381743));
#32415=CARTESIAN_POINT('Ctrl Pts',(2.04963761077958,-1.,-0.549938525150295));
#32416=CARTESIAN_POINT('Ctrl Pts',(2.04963761077958,1.,-0.549938525150295));
#32417=CARTESIAN_POINT('Ctrl Pts',(2.05427091604413,-1.,-0.554240657463906));
#32418=CARTESIAN_POINT('Ctrl Pts',(2.05427091604413,1.,-0.554240657463906));
#32419=CARTESIAN_POINT('Ctrl Pts',(2.05888537756462,-1.,-0.558579940185152));
#32420=CARTESIAN_POINT('Ctrl Pts',(2.05888537756462,1.,-0.558579940185152));
#32421=CARTESIAN_POINT('Ctrl Pts',(2.06348090160589,-1.,-0.562955993082262));
#32422=CARTESIAN_POINT('Ctrl Pts',(2.06348090160589,1.,-0.562955993082262));
#32423=CARTESIAN_POINT('Ctrl Pts',(2.06805732997334,-1.,-0.567368421181087));
#32424=CARTESIAN_POINT('Ctrl Pts',(2.06805732997334,1.,-0.567368421181087));
#32425=CARTESIAN_POINT('Ctrl Pts',(2.07261449292824,-1.,-0.571816823242603));
#32426=CARTESIAN_POINT('Ctrl Pts',(2.07261449292824,1.,-0.571816823242603));
#32427=CARTESIAN_POINT('Ctrl Pts',(2.07715226767559,-1.,-0.576300797416845));
#32428=CARTESIAN_POINT('Ctrl Pts',(2.07715226767559,1.,-0.576300797416845));
#32429=CARTESIAN_POINT('Ctrl Pts',(2.08167059018418,-1.,-0.580819952108064));
#32430=CARTESIAN_POINT('Ctrl Pts',(2.08167059018418,1.,-0.580819952108064));
#32431=CARTESIAN_POINT('Ctrl Pts',(2.08616943727951,-1.,-0.585373918991617));
#32432=CARTESIAN_POINT('Ctrl Pts',(2.08616943727951,1.,-0.585373918991617));
#32433=CARTESIAN_POINT('Ctrl Pts',(2.09064881812129,-1.,-0.589962365403406));
#32434=CARTESIAN_POINT('Ctrl Pts',(2.09064881812129,1.,-0.589962365403406));
#32435=CARTESIAN_POINT('Ctrl Pts',(2.0951087622027,-1.,-0.594585006052162));
#32436=CARTESIAN_POINT('Ctrl Pts',(2.0951087622027,1.,-0.594585006052162));
#32437=CARTESIAN_POINT('Ctrl Pts',(2.0995493086477,-1.,-0.599241616420534));
#32438=CARTESIAN_POINT('Ctrl Pts',(2.0995493086477,1.,-0.599241616420534));
#32439=CARTESIAN_POINT('Ctrl Pts',(2.10397049886949,-1.,-0.60393203073603));
#32440=CARTESIAN_POINT('Ctrl Pts',(2.10397049886949,1.,-0.60393203073603));
#32441=CARTESIAN_POINT('Ctrl Pts',(2.1074919961518,-1.,-0.607711315454876));
#32442=CARTESIAN_POINT('Ctrl Pts',(2.1074919961518,1.,-0.607711315454876));
#32443=CARTESIAN_POINT('Ctrl Pts',(2.11012443807238,-1.,-0.610560911689899));
#32444=CARTESIAN_POINT('Ctrl Pts',(2.11012443807238,1.,-0.610560911689899));
#32445=CARTESIAN_POINT('Ctrl Pts',(2.11187554259986,-1.,-0.6124673655618));
#32446=CARTESIAN_POINT('Ctrl Pts',(2.11187554259986,1.,-0.6124673655618));
#32447=CARTESIAN_POINT('Ctrl Pts',(2.11275013067528,-1.,-0.61342227326009));
#32448=CARTESIAN_POINT('Ctrl Pts',(2.11275013067528,1.,-0.61342227326009));
#32449=CARTESIAN_POINT('',(1.7075470150345,1.,-0.383122945602004));
#32450=CARTESIAN_POINT('Ctrl Pts',(1.7075470150345,1.,-0.383122945602004));
#32451=CARTESIAN_POINT('Ctrl Pts',(1.71231062891958,1.,-0.384119047315542));
#32452=CARTESIAN_POINT('Ctrl Pts',(1.72162022246158,1.,-0.38607079032701));
#32453=CARTESIAN_POINT('Ctrl Pts',(1.7349317097561,1.,-0.388877023509192));
#32454=CARTESIAN_POINT('Ctrl Pts',(1.75137405313962,1.,-0.392375812294307));
#32455=CARTESIAN_POINT('Ctrl Pts',(1.7697556004756,1.,-0.39634619612042));
#32456=CARTESIAN_POINT('Ctrl Pts',(1.78598826347533,1.,-0.399919403783081));
#32457=CARTESIAN_POINT('Ctrl Pts',(1.80012077176221,1.,-0.403107976170441));
#32458=CARTESIAN_POINT('Ctrl Pts',(1.81223801813988,1.,-0.405933518411838));
#32459=CARTESIAN_POINT('Ctrl Pts',(1.8224702267854,1.,-0.408428948108534));
#32460=CARTESIAN_POINT('Ctrl Pts',(1.83100408895216,1.,-0.410641256301675));
#32461=CARTESIAN_POINT('Ctrl Pts',(1.83808953475839,1.,-0.412633125322162));
#32462=CARTESIAN_POINT('Ctrl Pts',(1.8440575707371,1.,-0.41448743825434));
#32463=CARTESIAN_POINT('Ctrl Pts',(1.84929312929882,1.,-0.416300022038864));
#32464=CARTESIAN_POINT('Ctrl Pts',(1.85417632856234,1.,-0.418164129143534));
#32465=CARTESIAN_POINT('Ctrl Pts',(1.85903281096686,1.,-0.42015728797562));
#32466=CARTESIAN_POINT('Ctrl Pts',(1.86408083334028,1.,-0.422327307418275));
#32467=CARTESIAN_POINT('Ctrl Pts',(1.86937803944323,1.,-0.424678177291359));
#32468=CARTESIAN_POINT('Ctrl Pts',(1.87486989291484,1.,-0.427183828519102));
#32469=CARTESIAN_POINT('Ctrl Pts',(1.88044229001832,1.,-0.429803062482345));
#32470=CARTESIAN_POINT('Ctrl Pts',(1.88596913666793,1.,-0.432493038548748));
#32471=CARTESIAN_POINT('Ctrl Pts',(1.89136993975504,1.,-0.435225660963383));
#32472=CARTESIAN_POINT('Ctrl Pts',(1.89663648956466,1.,-0.437995003948244));
#32473=CARTESIAN_POINT('Ctrl Pts',(1.90180124389086,1.,-0.440807833704038));
#32474=CARTESIAN_POINT('Ctrl Pts',(1.90691756144898,1.,-0.443677556849151));
#32475=CARTESIAN_POINT('Ctrl Pts',(1.9120369998112,1.,-0.446617343485711));
#32476=CARTESIAN_POINT('Ctrl Pts',(1.91718342555755,1.,-0.449632260106662));
#32477=CARTESIAN_POINT('Ctrl Pts',(1.92235380648502,1.,-0.452719478359433));
#32478=CARTESIAN_POINT('Ctrl Pts',(1.92753067150476,1.,-0.455872005174371));
#32479=CARTESIAN_POINT('Ctrl Pts',(1.93269066517934,1.,-0.459081234547926));
#32480=CARTESIAN_POINT('Ctrl Pts',(1.93781486640821,1.,-0.462340031009057));
#32481=CARTESIAN_POINT('Ctrl Pts',(1.9428979419619,1.,-0.46564546202603));
#32482=CARTESIAN_POINT('Ctrl Pts',(1.94794381136514,1.,-0.468997482913135));
#32483=CARTESIAN_POINT('Ctrl Pts',(1.95296148278133,1.,-0.472397672264072));
#32484=CARTESIAN_POINT('Ctrl Pts',(1.95796111148177,1.,-0.475848034683176));
#32485=CARTESIAN_POINT('Ctrl Pts',(1.96294933055943,1.,-0.479349583074855));
#32486=CARTESIAN_POINT('Ctrl Pts',(1.96792703422362,1.,-0.482901662120691));
#32487=CARTESIAN_POINT('Ctrl Pts',(1.97289186263272,1.,-0.486502692907659));
#32488=CARTESIAN_POINT('Ctrl Pts',(1.97783973019229,1.,-0.490150627860953));
#32489=CARTESIAN_POINT('Ctrl Pts',(1.98276658761821,1.,-0.493843476541495));
#32490=CARTESIAN_POINT('Ctrl Pts',(1.98767044752932,1.,-0.497579909545574));
#32491=CARTESIAN_POINT('Ctrl Pts',(1.99255149126155,1.,-0.501359287727146));
#32492=CARTESIAN_POINT('Ctrl Pts',(1.99741107463572,1.,-0.505181361323026));
#32493=CARTESIAN_POINT('Ctrl Pts',(2.00225107134734,1.,-0.509046069886157));
#32494=CARTESIAN_POINT('Ctrl Pts',(2.00707309946949,1.,-0.512953306961793));
#32495=CARTESIAN_POINT('Ctrl Pts',(2.01187773939242,1.,-0.516902681728687));
#32496=CARTESIAN_POINT('Ctrl Pts',(2.01666477917286,1.,-0.520893590399371));
#32497=CARTESIAN_POINT('Ctrl Pts',(2.02143356304698,1.,-0.524925318333476));
#32498=CARTESIAN_POINT('Ctrl Pts',(2.0261832908329,1.,-0.528997127241914));
#32499=CARTESIAN_POINT('Ctrl Pts',(2.03091336214426,1.,-0.533108355132977));
#32500=CARTESIAN_POINT('Ctrl Pts',(2.03562362954037,1.,-0.537258489833262));
#32501=CARTESIAN_POINT('Ctrl Pts',(2.04031422690527,1.,-0.541447120615659));
#32502=CARTESIAN_POINT('Ctrl Pts',(2.04498544714588,1.,-0.54567390381743));
#32503=CARTESIAN_POINT('Ctrl Pts',(2.04963761077958,1.,-0.549938525150295));
#32504=CARTESIAN_POINT('Ctrl Pts',(2.05427091604413,1.,-0.554240657463906));
#32505=CARTESIAN_POINT('Ctrl Pts',(2.05888537756462,1.,-0.558579940185152));
#32506=CARTESIAN_POINT('Ctrl Pts',(2.06348090160589,1.,-0.562955993082262));
#32507=CARTESIAN_POINT('Ctrl Pts',(2.06805732997334,1.,-0.567368421181087));
#32508=CARTESIAN_POINT('Ctrl Pts',(2.07261449292824,1.,-0.571816823242603));
#32509=CARTESIAN_POINT('Ctrl Pts',(2.07715226767559,1.,-0.576300797416845));
#32510=CARTESIAN_POINT('Ctrl Pts',(2.08167059018418,1.,-0.580819952108064));
#32511=CARTESIAN_POINT('Ctrl Pts',(2.08616943727951,1.,-0.585373918991617));
#32512=CARTESIAN_POINT('Ctrl Pts',(2.09064881812129,1.,-0.589962365403406));
#32513=CARTESIAN_POINT('Ctrl Pts',(2.0951087622027,1.,-0.594585006052162));
#32514=CARTESIAN_POINT('Ctrl Pts',(2.0995493086477,1.,-0.599241616420534));
#32515=CARTESIAN_POINT('Ctrl Pts',(2.10397049886949,1.,-0.60393203073603));
#32516=CARTESIAN_POINT('Ctrl Pts',(2.1074919961518,1.,-0.607711315454876));
#32517=CARTESIAN_POINT('Ctrl Pts',(2.11012443807238,1.,-0.610560911689899));
#32518=CARTESIAN_POINT('Ctrl Pts',(2.11187554259986,1.,-0.6124673655618));
#32519=CARTESIAN_POINT('Ctrl Pts',(2.11275013067528,1.,-0.61342227326009));
#32520=CARTESIAN_POINT('',(1.7075470150345,0.,-0.383122945602001));
#32521=CARTESIAN_POINT('Origin',(0.,0.,0.));
#32522=CARTESIAN_POINT('',(1.74236521665491,1.,-0.163289472382896));
#32523=CARTESIAN_POINT('Origin',(0.,1.,0.));
#32524=CARTESIAN_POINT('',(1.74236521665491,0.,-0.163289472382896));
#32525=CARTESIAN_POINT('Ctrl Pts',(2.19890268624765,-1.,-0.0694764450219582));
#32526=CARTESIAN_POINT('Ctrl Pts',(2.19890268624765,1.,-0.0694764450219582));
#32527=CARTESIAN_POINT('Ctrl Pts',(2.19777582085423,-1.,-0.0701143536325491));
#32528=CARTESIAN_POINT('Ctrl Pts',(2.19777582085423,1.,-0.0701143536325491));
#32529=CARTESIAN_POINT('Ctrl Pts',(2.19552129484002,-1.,-0.0713863779526155));
#32530=CARTESIAN_POINT('Ctrl Pts',(2.19552129484002,1.,-0.0713863779526155));
#32531=CARTESIAN_POINT('Ctrl Pts',(2.19213712013662,-1.,-0.0732830357306726));
#32532=CARTESIAN_POINT('Ctrl Pts',(2.19213712013662,1.,-0.0732830357306726));
#32533=CARTESIAN_POINT('Ctrl Pts',(2.1876201139953,-1.,-0.0757891465836149));
#32534=CARTESIAN_POINT('Ctrl Pts',(2.1876201139953,1.,-0.0757891465836149));
#32535=CARTESIAN_POINT('Ctrl Pts',(2.18196589448887,-1.,-0.0788837727685244));
#32536=CARTESIAN_POINT('Ctrl Pts',(2.18196589448887,1.,-0.0788837727685244));
#32537=CARTESIAN_POINT('Ctrl Pts',(2.176303712113,-1.,-0.0819402680872767));
#32538=CARTESIAN_POINT('Ctrl Pts',(2.176303712113,1.,-0.0819402680872767));
#32539=CARTESIAN_POINT('Ctrl Pts',(2.17063357870952,-1.,-0.0849584620835374));
#32540=CARTESIAN_POINT('Ctrl Pts',(2.17063357870952,1.,-0.0849584620835374));
#32541=CARTESIAN_POINT('Ctrl Pts',(2.16495552645014,-1.,-0.0879381291386924));
#32542=CARTESIAN_POINT('Ctrl Pts',(2.16495552645014,1.,-0.0879381291386924));
#32543=CARTESIAN_POINT('Ctrl Pts',(2.15926961544516,-1.,-0.0908789888107267));
#32544=CARTESIAN_POINT('Ctrl Pts',(2.15926961544516,1.,-0.0908789888107267));
#32545=CARTESIAN_POINT('Ctrl Pts',(2.1535759397817,-1.,-0.0937807218867645));
#32546=CARTESIAN_POINT('Ctrl Pts',(2.1535759397817,1.,-0.0937807218867645));
#32547=CARTESIAN_POINT('Ctrl Pts',(2.14787463531795,-1.,-0.096642985230546));
#32548=CARTESIAN_POINT('Ctrl Pts',(2.14787463531795,1.,-0.096642985230546));
#32549=CARTESIAN_POINT('Ctrl Pts',(2.14216588396025,-1.,-0.0994654261990917));
#32550=CARTESIAN_POINT('Ctrl Pts',(2.14216588396025,1.,-0.0994654261990917));
#32551=CARTESIAN_POINT('Ctrl Pts',(2.13644992667165,-1.,-0.102247700556101));
#32552=CARTESIAN_POINT('Ctrl Pts',(2.13644992667165,1.,-0.102247700556101));
#32553=CARTESIAN_POINT('Ctrl Pts',(2.13072704887293,-1.,-0.10498947915274));
#32554=CARTESIAN_POINT('Ctrl Pts',(2.13072704887293,1.,-0.10498947915274));
#32555=CARTESIAN_POINT('Ctrl Pts',(2.12499752307,-1.,-0.10769043523109));
#32556=CARTESIAN_POINT('Ctrl Pts',(2.12499752307,1.,-0.10769043523109));
#32557=CARTESIAN_POINT('Ctrl Pts',(2.11926155590865,-1.,-0.110350236135025));
#32558=CARTESIAN_POINT('Ctrl Pts',(2.11926155590865,1.,-0.110350236135025));
#32559=CARTESIAN_POINT('Ctrl Pts',(2.11351924490306,-1.,-0.112968534419737));
#32560=CARTESIAN_POINT('Ctrl Pts',(2.11351924490306,1.,-0.112968534419737));
#32561=CARTESIAN_POINT('Ctrl Pts',(2.10777050261309,-1.,-0.115544957687927));
#32562=CARTESIAN_POINT('Ctrl Pts',(2.10777050261309,1.,-0.115544957687927));
#32563=CARTESIAN_POINT('Ctrl Pts',(2.102015121329,-1.,-0.118079107988356));
#32564=CARTESIAN_POINT('Ctrl Pts',(2.102015121329,1.,-0.118079107988356));
#32565=CARTESIAN_POINT('Ctrl Pts',(2.0962529286773,-1.,-0.120570567965122));
#32566=CARTESIAN_POINT('Ctrl Pts',(2.0962529286773,1.,-0.120570567965122));
#32567=CARTESIAN_POINT('Ctrl Pts',(2.09048392424825,-1.,-0.123018905621083));
#32568=CARTESIAN_POINT('Ctrl Pts',(2.09048392424825,1.,-0.123018905621083));
#32569=CARTESIAN_POINT('Ctrl Pts',(2.08470840653643,-1.,-0.125423679412062));
#32570=CARTESIAN_POINT('Ctrl Pts',(2.08470840653643,1.,-0.125423679412062));
#32571=CARTESIAN_POINT('Ctrl Pts',(2.07892715110987,-1.,-0.12778444527612));
#32572=CARTESIAN_POINT('Ctrl Pts',(2.07892715110987,1.,-0.12778444527612));
#32573=CARTESIAN_POINT('Ctrl Pts',(2.07314114713063,-1.,-0.130100748328404));
#32574=CARTESIAN_POINT('Ctrl Pts',(2.07314114713063,1.,-0.130100748328404));
#32575=CARTESIAN_POINT('Ctrl Pts',(2.06735123910326,-1.,-0.132372111547711));
#32576=CARTESIAN_POINT('Ctrl Pts',(2.06735123910326,1.,-0.132372111547711));
#32577=CARTESIAN_POINT('Ctrl Pts',(2.06155781517842,-1.,-0.134598026192106));
#32578=CARTESIAN_POINT('Ctrl Pts',(2.06155781517842,1.,-0.134598026192106));
#32579=CARTESIAN_POINT('Ctrl Pts',(2.05576044414264,-1.,-0.136777941218044));
#32580=CARTESIAN_POINT('Ctrl Pts',(2.05576044414264,1.,-0.136777941218044));
#32581=CARTESIAN_POINT('Ctrl Pts',(2.04995762001328,-1.,-0.138911255368966));
#32582=CARTESIAN_POINT('Ctrl Pts',(2.04995762001328,1.,-0.138911255368966));
#32583=CARTESIAN_POINT('Ctrl Pts',(2.04414757947916,-1.,-0.140997332152546));
#32584=CARTESIAN_POINT('Ctrl Pts',(2.04414757947916,1.,-0.140997332152546));
#32585=CARTESIAN_POINT('Ctrl Pts',(2.03832911025912,-1.,-0.143035515058209));
#32586=CARTESIAN_POINT('Ctrl Pts',(2.03832911025912,1.,-0.143035515058209));
#32587=CARTESIAN_POINT('Ctrl Pts',(2.03250223739942,-1.,-0.145025140186058));
#32588=CARTESIAN_POINT('Ctrl Pts',(2.03250223739942,1.,-0.145025140186058));
#32589=CARTESIAN_POINT('Ctrl Pts',(2.02666926182017,-1.,-0.146965557332583));
#32590=CARTESIAN_POINT('Ctrl Pts',(2.02666926182017,1.,-0.146965557332583));
#32591=CARTESIAN_POINT('Ctrl Pts',(2.02083464969894,-1.,-0.148856124775337));
#32592=CARTESIAN_POINT('Ctrl Pts',(2.02083464969894,1.,-0.148856124775337));
#32593=CARTESIAN_POINT('Ctrl Pts',(2.01500291940238,-1.,-0.150696157673078));
#32594=CARTESIAN_POINT('Ctrl Pts',(2.01500291940238,1.,-0.150696157673078));
#32595=CARTESIAN_POINT('Ctrl Pts',(2.00917680318424,-1.,-0.15248488362145));
#32596=CARTESIAN_POINT('Ctrl Pts',(2.00917680318424,1.,-0.15248488362145));
#32597=CARTESIAN_POINT('Ctrl Pts',(2.00335565310543,-1.,-0.154221403049722));
#32598=CARTESIAN_POINT('Ctrl Pts',(2.00335565310543,1.,-0.154221403049722));
#32599=CARTESIAN_POINT('Ctrl Pts',(1.99753284771497,-1.,-0.155904629548784));
#32600=CARTESIAN_POINT('Ctrl Pts',(1.99753284771497,1.,-0.155904629548784));
#32601=CARTESIAN_POINT('Ctrl Pts',(1.99169810931908,-1.,-0.157533331459227));
#32602=CARTESIAN_POINT('Ctrl Pts',(1.99169810931908,1.,-0.157533331459227));
#32603=CARTESIAN_POINT('Ctrl Pts',(1.98584238283292,-1.,-0.159106226437299));
#32604=CARTESIAN_POINT('Ctrl Pts',(1.98584238283292,1.,-0.159106226437299));
#32605=CARTESIAN_POINT('Ctrl Pts',(1.97996195437559,-1.,-0.160622060784611));
#32606=CARTESIAN_POINT('Ctrl Pts',(1.97996195437559,1.,-0.160622060784611));
#32607=CARTESIAN_POINT('Ctrl Pts',(1.97406280235188,-1.,-0.162079693556289));
#32608=CARTESIAN_POINT('Ctrl Pts',(1.97406280235188,1.,-0.162079693556289));
#32609=CARTESIAN_POINT('Ctrl Pts',(1.96816512677967,-1.,-0.163478185457734));
#32610=CARTESIAN_POINT('Ctrl Pts',(1.96816512677967,1.,-0.163478185457734));
#32611=CARTESIAN_POINT('Ctrl Pts',(1.96229379940136,-1.,-0.164816568920269));
#32612=CARTESIAN_POINT('Ctrl Pts',(1.96229379940136,1.,-0.164816568920269));
#32613=CARTESIAN_POINT('Ctrl Pts',(1.9564675971873,-1.,-0.166093592002813));
#32614=CARTESIAN_POINT('Ctrl Pts',(1.9564675971873,1.,-0.166093592002813));
#32615=CARTESIAN_POINT('Ctrl Pts',(1.95069027794294,-1.,-0.167307501784476));
#32616=CARTESIAN_POINT('Ctrl Pts',(1.95069027794294,1.,-0.167307501784476));
#32617=CARTESIAN_POINT('Ctrl Pts',(1.94493757756931,-1.,-0.168455741607556));
#32618=CARTESIAN_POINT('Ctrl Pts',(1.94493757756931,1.,-0.168455741607556));
#32619=CARTESIAN_POINT('Ctrl Pts',(1.93915639211581,-1.,-0.169534904817491));
#32620=CARTESIAN_POINT('Ctrl Pts',(1.93915639211581,1.,-0.169534904817491));
#32621=CARTESIAN_POINT('Ctrl Pts',(1.93329183155539,-1.,-0.170541253116202));
#32622=CARTESIAN_POINT('Ctrl Pts',(1.93329183155539,1.,-0.170541253116202));
#32623=CARTESIAN_POINT('Ctrl Pts',(1.92731093582036,-1.,-0.171471191532988));
#32624=CARTESIAN_POINT('Ctrl Pts',(1.92731093582036,1.,-0.171471191532988));
#32625=CARTESIAN_POINT('Ctrl Pts',(1.9212233439798,-1.,-0.172321621259514));
#32626=CARTESIAN_POINT('Ctrl Pts',(1.9212233439798,1.,-0.172321621259514));
#32627=CARTESIAN_POINT('Ctrl Pts',(1.91511429159527,-1.,-0.173090695383496));
#32628=CARTESIAN_POINT('Ctrl Pts',(1.91511429159527,1.,-0.173090695383496));
#32629=CARTESIAN_POINT('Ctrl Pts',(1.90911693975267,-1.,-0.173776635257817));
#32630=CARTESIAN_POINT('Ctrl Pts',(1.90911693975267,1.,-0.173776635257817));
#32631=CARTESIAN_POINT('Ctrl Pts',(1.90335253862834,-1.,-0.174375518661085));
#32632=CARTESIAN_POINT('Ctrl Pts',(1.90335253862834,1.,-0.174375518661085));
#32633=CARTESIAN_POINT('Ctrl Pts',(1.89788101117132,-1.,-0.174879405091263));
#32634=CARTESIAN_POINT('Ctrl Pts',(1.89788101117132,1.,-0.174879405091263));
#32635=CARTESIAN_POINT('Ctrl Pts',(1.892646301985,-1.,-0.175274276190844));
#32636=CARTESIAN_POINT('Ctrl Pts',(1.892646301985,1.,-0.175274276190844));
#32637=CARTESIAN_POINT('Ctrl Pts',(1.88742606273259,-1.,-0.175538155840648));
#32638=CARTESIAN_POINT('Ctrl Pts',(1.88742606273259,1.,-0.175538155840648));
#32639=CARTESIAN_POINT('Ctrl Pts',(1.88188663145367,-1.,-0.175644148889699));
#32640=CARTESIAN_POINT('Ctrl Pts',(1.88188663145367,1.,-0.175644148889699));
#32641=CARTESIAN_POINT('Ctrl Pts',(1.87563767773588,-1.,-0.175563480746485));
#32642=CARTESIAN_POINT('Ctrl Pts',(1.87563767773588,1.,-0.175563480746485));
#32643=CARTESIAN_POINT('Ctrl Pts',(1.86828349694799,-1.,-0.175268337590758));
#32644=CARTESIAN_POINT('Ctrl Pts',(1.86828349694799,1.,-0.175268337590758));
#32645=CARTESIAN_POINT('Ctrl Pts',(1.85948367088837,-1.,-0.17473525927603));
#32646=CARTESIAN_POINT('Ctrl Pts',(1.85948367088837,1.,-0.17473525927603));
#32647=CARTESIAN_POINT('Ctrl Pts',(1.8489811319852,-1.,-0.173946627587732));
#32648=CARTESIAN_POINT('Ctrl Pts',(1.8489811319852,1.,-0.173946627587732));
#32649=CARTESIAN_POINT('Ctrl Pts',(1.83658380527692,-1.,-0.1728894428919));
#32650=CARTESIAN_POINT('Ctrl Pts',(1.83658380527692,1.,-0.1728894428919));
#32651=CARTESIAN_POINT('Ctrl Pts',(1.82215766811545,-1.,-0.171554770204119));
#32652=CARTESIAN_POINT('Ctrl Pts',(1.82215766811545,1.,-0.171554770204119));
#32653=CARTESIAN_POINT('Ctrl Pts',(1.80561530629706,-1.,-0.169936923904608));
#32654=CARTESIAN_POINT('Ctrl Pts',(1.80561530629706,1.,-0.169936923904608));
#32655=CARTESIAN_POINT('Ctrl Pts',(1.7869064998507,-1.,-0.168032772805197));
#32656=CARTESIAN_POINT('Ctrl Pts',(1.7869064998507,1.,-0.168032772805197));
#32657=CARTESIAN_POINT('Ctrl Pts',(1.77018771684844,-1.,-0.1662793551464));
#32658=CARTESIAN_POINT('Ctrl Pts',(1.77018771684844,1.,-0.1662793551464));
#32659=CARTESIAN_POINT('Ctrl Pts',(1.75666056638427,-1.,-0.164834765707159));
#32660=CARTESIAN_POINT('Ctrl Pts',(1.75666056638427,1.,-0.164834765707159));
#32661=CARTESIAN_POINT('Ctrl Pts',(1.7472034950333,-1.,-0.163814161002002));
#32662=CARTESIAN_POINT('Ctrl Pts',(1.7472034950333,1.,-0.163814161002002));
#32663=CARTESIAN_POINT('Ctrl Pts',(1.74236521665491,-1.,-0.163289472382896));
#32664=CARTESIAN_POINT('Ctrl Pts',(1.74236521665491,1.,-0.163289472382896));
#32665=CARTESIAN_POINT('',(2.19890268624765,1.,-0.0694764450219582));
#32666=CARTESIAN_POINT('Ctrl Pts',(2.19890268624765,1.,-0.0694764450219582));
#32667=CARTESIAN_POINT('Ctrl Pts',(2.19777582085423,1.,-0.0701143536325491));
#32668=CARTESIAN_POINT('Ctrl Pts',(2.19552129484002,1.,-0.0713863779526155));
#32669=CARTESIAN_POINT('Ctrl Pts',(2.19213712013662,1.,-0.0732830357306726));
#32670=CARTESIAN_POINT('Ctrl Pts',(2.1876201139953,1.,-0.0757891465836149));
#32671=CARTESIAN_POINT('Ctrl Pts',(2.18196589448887,1.,-0.0788837727685244));
#32672=CARTESIAN_POINT('Ctrl Pts',(2.176303712113,1.,-0.0819402680872767));
#32673=CARTESIAN_POINT('Ctrl Pts',(2.17063357870952,1.,-0.0849584620835374));
#32674=CARTESIAN_POINT('Ctrl Pts',(2.16495552645014,1.,-0.0879381291386924));
#32675=CARTESIAN_POINT('Ctrl Pts',(2.15926961544516,1.,-0.0908789888107267));
#32676=CARTESIAN_POINT('Ctrl Pts',(2.1535759397817,1.,-0.0937807218867645));
#32677=CARTESIAN_POINT('Ctrl Pts',(2.14787463531795,1.,-0.096642985230546));
#32678=CARTESIAN_POINT('Ctrl Pts',(2.14216588396025,1.,-0.0994654261990917));
#32679=CARTESIAN_POINT('Ctrl Pts',(2.13644992667165,1.,-0.102247700556101));
#32680=CARTESIAN_POINT('Ctrl Pts',(2.13072704887293,1.,-0.10498947915274));
#32681=CARTESIAN_POINT('Ctrl Pts',(2.12499752307,1.,-0.10769043523109));
#32682=CARTESIAN_POINT('Ctrl Pts',(2.11926155590865,1.,-0.110350236135025));
#32683=CARTESIAN_POINT('Ctrl Pts',(2.11351924490306,1.,-0.112968534419737));
#32684=CARTESIAN_POINT('Ctrl Pts',(2.10777050261309,1.,-0.115544957687927));
#32685=CARTESIAN_POINT('Ctrl Pts',(2.102015121329,1.,-0.118079107988356));
#32686=CARTESIAN_POINT('Ctrl Pts',(2.0962529286773,1.,-0.120570567965122));
#32687=CARTESIAN_POINT('Ctrl Pts',(2.09048392424825,1.,-0.123018905621083));
#32688=CARTESIAN_POINT('Ctrl Pts',(2.08470840653643,1.,-0.125423679412062));
#32689=CARTESIAN_POINT('Ctrl Pts',(2.07892715110987,1.,-0.12778444527612));
#32690=CARTESIAN_POINT('Ctrl Pts',(2.07314114713063,1.,-0.130100748328404));
#32691=CARTESIAN_POINT('Ctrl Pts',(2.06735123910326,1.,-0.132372111547711));
#32692=CARTESIAN_POINT('Ctrl Pts',(2.06155781517842,1.,-0.134598026192106));
#32693=CARTESIAN_POINT('Ctrl Pts',(2.05576044414264,1.,-0.136777941218044));
#32694=CARTESIAN_POINT('Ctrl Pts',(2.04995762001328,1.,-0.138911255368966));
#32695=CARTESIAN_POINT('Ctrl Pts',(2.04414757947916,1.,-0.140997332152546));
#32696=CARTESIAN_POINT('Ctrl Pts',(2.03832911025912,1.,-0.143035515058209));
#32697=CARTESIAN_POINT('Ctrl Pts',(2.03250223739942,1.,-0.145025140186058));
#32698=CARTESIAN_POINT('Ctrl Pts',(2.02666926182017,1.,-0.146965557332583));
#32699=CARTESIAN_POINT('Ctrl Pts',(2.02083464969894,1.,-0.148856124775337));
#32700=CARTESIAN_POINT('Ctrl Pts',(2.01500291940238,1.,-0.150696157673078));
#32701=CARTESIAN_POINT('Ctrl Pts',(2.00917680318424,1.,-0.15248488362145));
#32702=CARTESIAN_POINT('Ctrl Pts',(2.00335565310543,1.,-0.154221403049722));
#32703=CARTESIAN_POINT('Ctrl Pts',(1.99753284771497,1.,-0.155904629548784));
#32704=CARTESIAN_POINT('Ctrl Pts',(1.99169810931908,1.,-0.157533331459227));
#32705=CARTESIAN_POINT('Ctrl Pts',(1.98584238283292,1.,-0.159106226437299));
#32706=CARTESIAN_POINT('Ctrl Pts',(1.97996195437559,1.,-0.160622060784611));
#32707=CARTESIAN_POINT('Ctrl Pts',(1.97406280235188,1.,-0.162079693556289));
#32708=CARTESIAN_POINT('Ctrl Pts',(1.96816512677967,1.,-0.163478185457734));
#32709=CARTESIAN_POINT('Ctrl Pts',(1.96229379940136,1.,-0.164816568920269));
#32710=CARTESIAN_POINT('Ctrl Pts',(1.9564675971873,1.,-0.166093592002813));
#32711=CARTESIAN_POINT('Ctrl Pts',(1.95069027794294,1.,-0.167307501784476));
#32712=CARTESIAN_POINT('Ctrl Pts',(1.94493757756931,1.,-0.168455741607556));
#32713=CARTESIAN_POINT('Ctrl Pts',(1.93915639211581,1.,-0.169534904817491));
#32714=CARTESIAN_POINT('Ctrl Pts',(1.93329183155539,1.,-0.170541253116202));
#32715=CARTESIAN_POINT('Ctrl Pts',(1.92731093582036,1.,-0.171471191532988));
#32716=CARTESIAN_POINT('Ctrl Pts',(1.9212233439798,1.,-0.172321621259514));
#32717=CARTESIAN_POINT('Ctrl Pts',(1.91511429159527,1.,-0.173090695383496));
#32718=CARTESIAN_POINT('Ctrl Pts',(1.90911693975267,1.,-0.173776635257817));
#32719=CARTESIAN_POINT('Ctrl Pts',(1.90335253862834,1.,-0.174375518661085));
#32720=CARTESIAN_POINT('Ctrl Pts',(1.89788101117132,1.,-0.174879405091263));
#32721=CARTESIAN_POINT('Ctrl Pts',(1.892646301985,1.,-0.175274276190844));
#32722=CARTESIAN_POINT('Ctrl Pts',(1.88742606273259,1.,-0.175538155840648));
#32723=CARTESIAN_POINT('Ctrl Pts',(1.88188663145367,1.,-0.175644148889699));
#32724=CARTESIAN_POINT('Ctrl Pts',(1.87563767773588,1.,-0.175563480746485));
#32725=CARTESIAN_POINT('Ctrl Pts',(1.86828349694799,1.,-0.175268337590758));
#32726=CARTESIAN_POINT('Ctrl Pts',(1.85948367088837,1.,-0.17473525927603));
#32727=CARTESIAN_POINT('Ctrl Pts',(1.8489811319852,1.,-0.173946627587732));
#32728=CARTESIAN_POINT('Ctrl Pts',(1.83658380527692,1.,-0.1728894428919));
#32729=CARTESIAN_POINT('Ctrl Pts',(1.82215766811545,1.,-0.171554770204119));
#32730=CARTESIAN_POINT('Ctrl Pts',(1.80561530629706,1.,-0.169936923904608));
#32731=CARTESIAN_POINT('Ctrl Pts',(1.7869064998507,1.,-0.168032772805197));
#32732=CARTESIAN_POINT('Ctrl Pts',(1.77018771684844,1.,-0.1662793551464));
#32733=CARTESIAN_POINT('Ctrl Pts',(1.75666056638427,1.,-0.164834765707159));
#32734=CARTESIAN_POINT('Ctrl Pts',(1.7472034950333,1.,-0.163814161002002));
#32735=CARTESIAN_POINT('Ctrl Pts',(1.74236521665491,1.,-0.163289472382896));
#32736=CARTESIAN_POINT('',(2.19890268624765,0.,-0.0694764450219582));
#32737=CARTESIAN_POINT('Origin',(2.19890268624765,0.,0.0694764450219582));
#32738=CARTESIAN_POINT('',(2.19890268624765,1.,0.0694764450219582));
#32739=CARTESIAN_POINT('',(2.19890268624765,1.,-0.0694764450219582));
#32740=CARTESIAN_POINT('',(2.19890268624765,0.,0.0694764450219582));
#32741=CARTESIAN_POINT('Ctrl Pts',(1.74236521665491,-1.,0.163289472382896));
#32742=CARTESIAN_POINT('Ctrl Pts',(1.74236521665491,1.,0.163289472382896));
#32743=CARTESIAN_POINT('Ctrl Pts',(1.74720349503904,-1.,0.163814161002474));
#32744=CARTESIAN_POINT('Ctrl Pts',(1.74720349503904,1.,0.163814161002474));
#32745=CARTESIAN_POINT('Ctrl Pts',(1.75666056640041,-1.,0.164834765708484));
#32746=CARTESIAN_POINT('Ctrl Pts',(1.75666056640041,1.,0.164834765708484));
#32747=CARTESIAN_POINT('Ctrl Pts',(1.77018771687692,-1.,0.166279355148738));
#32748=CARTESIAN_POINT('Ctrl Pts',(1.77018771687692,1.,0.166279355148738));
#32749=CARTESIAN_POINT('Ctrl Pts',(1.78690649988931,-1.,0.16803277280837));
#32750=CARTESIAN_POINT('Ctrl Pts',(1.78690649988931,1.,0.16803277280837));
#32751=CARTESIAN_POINT('Ctrl Pts',(1.80561530633924,-1.,0.169936923908078));
#32752=CARTESIAN_POINT('Ctrl Pts',(1.80561530633924,1.,0.169936923908078));
#32753=CARTESIAN_POINT('Ctrl Pts',(1.82215766815414,-1.,0.171554770207306));
#32754=CARTESIAN_POINT('Ctrl Pts',(1.82215766815414,1.,0.171554770207306));
#32755=CARTESIAN_POINT('Ctrl Pts',(1.83658380530747,-1.,0.17288944289442));
#32756=CARTESIAN_POINT('Ctrl Pts',(1.83658380530747,1.,0.17288944289442));
#32757=CARTESIAN_POINT('Ctrl Pts',(1.84898113200543,-1.,0.173946627589401));
#32758=CARTESIAN_POINT('Ctrl Pts',(1.84898113200543,1.,0.173946627589401));
#32759=CARTESIAN_POINT('Ctrl Pts',(1.85948367089838,-1.,0.174735259276856));
#32760=CARTESIAN_POINT('Ctrl Pts',(1.85948367089838,1.,0.174735259276856));
#32761=CARTESIAN_POINT('Ctrl Pts',(1.86828349694972,-1.,0.1752683375909));
#32762=CARTESIAN_POINT('Ctrl Pts',(1.86828349694972,1.,0.1752683375909));
#32763=CARTESIAN_POINT('Ctrl Pts',(1.87563767773249,-1.,0.175563480746205));
#32764=CARTESIAN_POINT('Ctrl Pts',(1.87563767773249,1.,0.175563480746205));
#32765=CARTESIAN_POINT('Ctrl Pts',(1.88188663144846,-1.,0.175644148889271));
#32766=CARTESIAN_POINT('Ctrl Pts',(1.88188663144846,1.,0.175644148889271));
#32767=CARTESIAN_POINT('Ctrl Pts',(1.88742606272818,-1.,0.175538155840286));
#32768=CARTESIAN_POINT('Ctrl Pts',(1.88742606272818,1.,0.175538155840286));
#32769=CARTESIAN_POINT('Ctrl Pts',(1.89264630198279,-1.,0.175274276190664));
#32770=CARTESIAN_POINT('Ctrl Pts',(1.89264630198279,1.,0.175274276190664));
#32771=CARTESIAN_POINT('Ctrl Pts',(1.89788101117148,-1.,0.174879405091277));
#32772=CARTESIAN_POINT('Ctrl Pts',(1.89788101117148,1.,0.174879405091277));
#32773=CARTESIAN_POINT('Ctrl Pts',(1.90335253863003,-1.,0.174375518661222));
#32774=CARTESIAN_POINT('Ctrl Pts',(1.90335253863003,1.,0.174375518661222));
#32775=CARTESIAN_POINT('Ctrl Pts',(1.90911693975475,-1.,0.173776635257983));
#32776=CARTESIAN_POINT('Ctrl Pts',(1.90911693975475,1.,0.173776635257983));
#32777=CARTESIAN_POINT('Ctrl Pts',(1.91511429159681,-1.,0.173090695383619));
#32778=CARTESIAN_POINT('Ctrl Pts',(1.91511429159681,1.,0.173090695383619));
#32779=CARTESIAN_POINT('Ctrl Pts',(1.92122334398034,-1.,0.172321621259556));
#32780=CARTESIAN_POINT('Ctrl Pts',(1.92122334398034,1.,0.172321621259556));
#32781=CARTESIAN_POINT('Ctrl Pts',(1.92731093582,-1.,0.17147119153296));
#32782=CARTESIAN_POINT('Ctrl Pts',(1.92731093582,1.,0.17147119153296));
#32783=CARTESIAN_POINT('Ctrl Pts',(1.93329183155455,-1.,0.170541253116136));
#32784=CARTESIAN_POINT('Ctrl Pts',(1.93329183155455,1.,0.170541253116136));
#32785=CARTESIAN_POINT('Ctrl Pts',(1.93915639211497,-1.,0.169534904817425));
#32786=CARTESIAN_POINT('Ctrl Pts',(1.93915639211497,1.,0.169534904817425));
#32787=CARTESIAN_POINT('Ctrl Pts',(1.94493757756879,-1.,0.168455741607515));
#32788=CARTESIAN_POINT('Ctrl Pts',(1.94493757756879,1.,0.168455741607515));
#32789=CARTESIAN_POINT('Ctrl Pts',(1.95069027794286,-1.,0.167307501784469));
#32790=CARTESIAN_POINT('Ctrl Pts',(1.95069027794286,1.,0.167307501784469));
#32791=CARTESIAN_POINT('Ctrl Pts',(1.95646759718755,-1.,0.166093592002832));
#32792=CARTESIAN_POINT('Ctrl Pts',(1.95646759718755,1.,0.166093592002832));
#32793=CARTESIAN_POINT('Ctrl Pts',(1.96229379940174,-1.,0.1648165689203));
#32794=CARTESIAN_POINT('Ctrl Pts',(1.96229379940174,1.,0.1648165689203));
#32795=CARTESIAN_POINT('Ctrl Pts',(1.96816512678,-1.,0.16347818545776));
#32796=CARTESIAN_POINT('Ctrl Pts',(1.96816512678,1.,0.16347818545776));
#32797=CARTESIAN_POINT('Ctrl Pts',(1.97406280235204,-1.,0.162079693556302));
#32798=CARTESIAN_POINT('Ctrl Pts',(1.97406280235204,1.,0.162079693556302));
#32799=CARTESIAN_POINT('Ctrl Pts',(1.97996195437557,-1.,0.16062206078461));
#32800=CARTESIAN_POINT('Ctrl Pts',(1.97996195437557,1.,0.16062206078461));
#32801=CARTESIAN_POINT('Ctrl Pts',(1.98584238283279,-1.,0.159106226437288));
#32802=CARTESIAN_POINT('Ctrl Pts',(1.98584238283279,1.,0.159106226437288));
#32803=CARTESIAN_POINT('Ctrl Pts',(1.99169810931893,-1.,0.157533331459215));
#32804=CARTESIAN_POINT('Ctrl Pts',(1.99169810931893,1.,0.157533331459215));
#32805=CARTESIAN_POINT('Ctrl Pts',(1.99753284771487,-1.,0.155904629548774));
#32806=CARTESIAN_POINT('Ctrl Pts',(1.99753284771487,1.,0.155904629548774));
#32807=CARTESIAN_POINT('Ctrl Pts',(2.00335565310539,-1.,0.154221403049719));
#32808=CARTESIAN_POINT('Ctrl Pts',(2.00335565310539,1.,0.154221403049719));
#32809=CARTESIAN_POINT('Ctrl Pts',(2.00917680318426,-1.,0.152484883621452));
#32810=CARTESIAN_POINT('Ctrl Pts',(2.00917680318426,1.,0.152484883621452));
#32811=CARTESIAN_POINT('Ctrl Pts',(2.01500291940243,-1.,0.150696157673084));
#32812=CARTESIAN_POINT('Ctrl Pts',(2.01500291940243,1.,0.150696157673084));
#32813=CARTESIAN_POINT('Ctrl Pts',(2.02083464969897,-1.,0.148856124775342));
#32814=CARTESIAN_POINT('Ctrl Pts',(2.02083464969897,1.,0.148856124775342));
#32815=CARTESIAN_POINT('Ctrl Pts',(2.02666926182017,-1.,0.146965557332586));
#32816=CARTESIAN_POINT('Ctrl Pts',(2.02666926182017,1.,0.146965557332586));
#32817=CARTESIAN_POINT('Ctrl Pts',(2.03250223739941,-1.,0.145025140186058));
#32818=CARTESIAN_POINT('Ctrl Pts',(2.03250223739941,1.,0.145025140186058));
#32819=CARTESIAN_POINT('Ctrl Pts',(2.03832911025913,-1.,0.143035515058208));
#32820=CARTESIAN_POINT('Ctrl Pts',(2.03832911025913,1.,0.143035515058208));
#32821=CARTESIAN_POINT('Ctrl Pts',(2.04414757947919,-1.,0.140997332152545));
#32822=CARTESIAN_POINT('Ctrl Pts',(2.04414757947919,1.,0.140997332152545));
#32823=CARTESIAN_POINT('Ctrl Pts',(2.04995762001333,-1.,0.138911255368966));
#32824=CARTESIAN_POINT('Ctrl Pts',(2.04995762001333,1.,0.138911255368966));
#32825=CARTESIAN_POINT('Ctrl Pts',(2.0557604441427,-1.,0.136777941218044));
#32826=CARTESIAN_POINT('Ctrl Pts',(2.0557604441427,1.,0.136777941218044));
#32827=CARTESIAN_POINT('Ctrl Pts',(2.06155781517844,-1.,0.134598026192107));
#32828=CARTESIAN_POINT('Ctrl Pts',(2.06155781517844,1.,0.134598026192107));
#32829=CARTESIAN_POINT('Ctrl Pts',(2.06735123910319,-1.,0.132372111547709));
#32830=CARTESIAN_POINT('Ctrl Pts',(2.06735123910319,1.,0.132372111547709));
#32831=CARTESIAN_POINT('Ctrl Pts',(2.07314114713047,-1.,0.1301007483284));
#32832=CARTESIAN_POINT('Ctrl Pts',(2.07314114713047,1.,0.1301007483284));
#32833=CARTESIAN_POINT('Ctrl Pts',(2.07892715110967,-1.,0.127784445276116));
#32834=CARTESIAN_POINT('Ctrl Pts',(2.07892715110967,1.,0.127784445276116));
#32835=CARTESIAN_POINT('Ctrl Pts',(2.08470840653628,-1.,0.125423679412058));
#32836=CARTESIAN_POINT('Ctrl Pts',(2.08470840653628,1.,0.125423679412058));
#32837=CARTESIAN_POINT('Ctrl Pts',(2.09048392424826,-1.,0.123018905621083));
#32838=CARTESIAN_POINT('Ctrl Pts',(2.09048392424826,1.,0.123018905621083));
#32839=CARTESIAN_POINT('Ctrl Pts',(2.09625292867756,-1.,0.120570567965129));
#32840=CARTESIAN_POINT('Ctrl Pts',(2.09625292867756,1.,0.120570567965129));
#32841=CARTESIAN_POINT('Ctrl Pts',(2.10201512132945,-1.,0.118079107988368));
#32842=CARTESIAN_POINT('Ctrl Pts',(2.10201512132945,1.,0.118079107988368));
#32843=CARTESIAN_POINT('Ctrl Pts',(2.10777050261359,-1.,0.11554495768794));
#32844=CARTESIAN_POINT('Ctrl Pts',(2.10777050261359,1.,0.11554495768794));
#32845=CARTESIAN_POINT('Ctrl Pts',(2.11351924490335,-1.,0.112968534419746));
#32846=CARTESIAN_POINT('Ctrl Pts',(2.11351924490335,1.,0.112968534419746));
#32847=CARTESIAN_POINT('Ctrl Pts',(2.11926155590849,-1.,0.11035023613502));
#32848=CARTESIAN_POINT('Ctrl Pts',(2.11926155590849,1.,0.11035023613502));
#32849=CARTESIAN_POINT('Ctrl Pts',(2.12499752306927,-1.,0.107690435231068));
#32850=CARTESIAN_POINT('Ctrl Pts',(2.12499752306927,1.,0.107690435231068));
#32851=CARTESIAN_POINT('Ctrl Pts',(2.1307270488718,-1.,0.104989479152703));
#32852=CARTESIAN_POINT('Ctrl Pts',(2.1307270488718,1.,0.104989479152703));
#32853=CARTESIAN_POINT('Ctrl Pts',(2.13644992667052,-1.,0.102247700556063));
#32854=CARTESIAN_POINT('Ctrl Pts',(2.13644992667052,1.,0.102247700556063));
#32855=CARTESIAN_POINT('Ctrl Pts',(2.14216588395974,-1.,0.0994654261990741));
#32856=CARTESIAN_POINT('Ctrl Pts',(2.14216588395974,1.,0.0994654261990741));
#32857=CARTESIAN_POINT('Ctrl Pts',(2.14787463531864,-1.,0.0966429852305688));
#32858=CARTESIAN_POINT('Ctrl Pts',(2.14787463531864,1.,0.0966429852305688));
#32859=CARTESIAN_POINT('Ctrl Pts',(2.15357593978377,-1.,0.0937807218868344));
#32860=CARTESIAN_POINT('Ctrl Pts',(2.15357593978377,1.,0.0937807218868344));
#32861=CARTESIAN_POINT('Ctrl Pts',(2.15926961544808,-1.,0.0908789888108265));
#32862=CARTESIAN_POINT('Ctrl Pts',(2.15926961544808,1.,0.0908789888108265));
#32863=CARTESIAN_POINT('Ctrl Pts',(2.16495552645275,-1.,0.0879381291387821));
#32864=CARTESIAN_POINT('Ctrl Pts',(2.16495552645275,1.,0.0879381291387821));
#32865=CARTESIAN_POINT('Ctrl Pts',(2.17063357871031,-1.,0.0849584620835642));
#32866=CARTESIAN_POINT('Ctrl Pts',(2.17063357871031,1.,0.0849584620835642));
#32867=CARTESIAN_POINT('Ctrl Pts',(2.1763037121106,-1.,0.0819402680871938));
#32868=CARTESIAN_POINT('Ctrl Pts',(2.1763037121106,1.,0.0819402680871938));
#32869=CARTESIAN_POINT('Ctrl Pts',(2.18196589448304,-1.,0.0788837727683226));
#32870=CARTESIAN_POINT('Ctrl Pts',(2.18196589448304,1.,0.0788837727683226));
#32871=CARTESIAN_POINT('Ctrl Pts',(2.1876201139874,-1.,0.075789146583341));
#32872=CARTESIAN_POINT('Ctrl Pts',(2.1876201139874,1.,0.075789146583341));
#32873=CARTESIAN_POINT('Ctrl Pts',(2.19213712012956,-1.,0.0732830357304275));
#32874=CARTESIAN_POINT('Ctrl Pts',(2.19213712012956,1.,0.0732830357304275));
#32875=CARTESIAN_POINT('Ctrl Pts',(2.19552129483562,-1.,0.0713863779524626));
#32876=CARTESIAN_POINT('Ctrl Pts',(2.19552129483562,1.,0.0713863779524626));
#32877=CARTESIAN_POINT('Ctrl Pts',(2.19777582085261,-1.,0.0701143536324925));
#32878=CARTESIAN_POINT('Ctrl Pts',(2.19777582085261,1.,0.0701143536324925));
#32879=CARTESIAN_POINT('Ctrl Pts',(2.19890268624765,-1.,0.0694764450219582));
#32880=CARTESIAN_POINT('Ctrl Pts',(2.19890268624765,1.,0.0694764450219582));
#32881=CARTESIAN_POINT('',(1.74236521665491,1.,0.163289472382896));
#32882=CARTESIAN_POINT('Ctrl Pts',(1.74236521665491,1.,0.163289472382896));
#32883=CARTESIAN_POINT('Ctrl Pts',(1.74720349503904,1.,0.163814161002474));
#32884=CARTESIAN_POINT('Ctrl Pts',(1.75666056640041,1.,0.164834765708484));
#32885=CARTESIAN_POINT('Ctrl Pts',(1.77018771687692,1.,0.166279355148738));
#32886=CARTESIAN_POINT('Ctrl Pts',(1.78690649988931,1.,0.16803277280837));
#32887=CARTESIAN_POINT('Ctrl Pts',(1.80561530633924,1.,0.169936923908078));
#32888=CARTESIAN_POINT('Ctrl Pts',(1.82215766815414,1.,0.171554770207306));
#32889=CARTESIAN_POINT('Ctrl Pts',(1.83658380530747,1.,0.17288944289442));
#32890=CARTESIAN_POINT('Ctrl Pts',(1.84898113200543,1.,0.173946627589401));
#32891=CARTESIAN_POINT('Ctrl Pts',(1.85948367089838,1.,0.174735259276856));
#32892=CARTESIAN_POINT('Ctrl Pts',(1.86828349694972,1.,0.1752683375909));
#32893=CARTESIAN_POINT('Ctrl Pts',(1.87563767773249,1.,0.175563480746205));
#32894=CARTESIAN_POINT('Ctrl Pts',(1.88188663144846,1.,0.175644148889271));
#32895=CARTESIAN_POINT('Ctrl Pts',(1.88742606272818,1.,0.175538155840286));
#32896=CARTESIAN_POINT('Ctrl Pts',(1.89264630198279,1.,0.175274276190664));
#32897=CARTESIAN_POINT('Ctrl Pts',(1.89788101117148,1.,0.174879405091277));
#32898=CARTESIAN_POINT('Ctrl Pts',(1.90335253863003,1.,0.174375518661222));
#32899=CARTESIAN_POINT('Ctrl Pts',(1.90911693975475,1.,0.173776635257983));
#32900=CARTESIAN_POINT('Ctrl Pts',(1.91511429159681,1.,0.173090695383619));
#32901=CARTESIAN_POINT('Ctrl Pts',(1.92122334398034,1.,0.172321621259556));
#32902=CARTESIAN_POINT('Ctrl Pts',(1.92731093582,1.,0.17147119153296));
#32903=CARTESIAN_POINT('Ctrl Pts',(1.93329183155455,1.,0.170541253116136));
#32904=CARTESIAN_POINT('Ctrl Pts',(1.93915639211497,1.,0.169534904817425));
#32905=CARTESIAN_POINT('Ctrl Pts',(1.94493757756879,1.,0.168455741607515));
#32906=CARTESIAN_POINT('Ctrl Pts',(1.95069027794286,1.,0.167307501784469));
#32907=CARTESIAN_POINT('Ctrl Pts',(1.95646759718755,1.,0.166093592002832));
#32908=CARTESIAN_POINT('Ctrl Pts',(1.96229379940174,1.,0.1648165689203));
#32909=CARTESIAN_POINT('Ctrl Pts',(1.96816512678,1.,0.16347818545776));
#32910=CARTESIAN_POINT('Ctrl Pts',(1.97406280235204,1.,0.162079693556302));
#32911=CARTESIAN_POINT('Ctrl Pts',(1.97996195437557,1.,0.16062206078461));
#32912=CARTESIAN_POINT('Ctrl Pts',(1.98584238283279,1.,0.159106226437288));
#32913=CARTESIAN_POINT('Ctrl Pts',(1.99169810931893,1.,0.157533331459215));
#32914=CARTESIAN_POINT('Ctrl Pts',(1.99753284771487,1.,0.155904629548774));
#32915=CARTESIAN_POINT('Ctrl Pts',(2.00335565310539,1.,0.154221403049719));
#32916=CARTESIAN_POINT('Ctrl Pts',(2.00917680318426,1.,0.152484883621452));
#32917=CARTESIAN_POINT('Ctrl Pts',(2.01500291940243,1.,0.150696157673084));
#32918=CARTESIAN_POINT('Ctrl Pts',(2.02083464969897,1.,0.148856124775342));
#32919=CARTESIAN_POINT('Ctrl Pts',(2.02666926182017,1.,0.146965557332586));
#32920=CARTESIAN_POINT('Ctrl Pts',(2.03250223739941,1.,0.145025140186058));
#32921=CARTESIAN_POINT('Ctrl Pts',(2.03832911025913,1.,0.143035515058208));
#32922=CARTESIAN_POINT('Ctrl Pts',(2.04414757947919,1.,0.140997332152545));
#32923=CARTESIAN_POINT('Ctrl Pts',(2.04995762001333,1.,0.138911255368966));
#32924=CARTESIAN_POINT('Ctrl Pts',(2.0557604441427,1.,0.136777941218044));
#32925=CARTESIAN_POINT('Ctrl Pts',(2.06155781517844,1.,0.134598026192107));
#32926=CARTESIAN_POINT('Ctrl Pts',(2.06735123910319,1.,0.132372111547709));
#32927=CARTESIAN_POINT('Ctrl Pts',(2.07314114713047,1.,0.1301007483284));
#32928=CARTESIAN_POINT('Ctrl Pts',(2.07892715110967,1.,0.127784445276116));
#32929=CARTESIAN_POINT('Ctrl Pts',(2.08470840653628,1.,0.125423679412058));
#32930=CARTESIAN_POINT('Ctrl Pts',(2.09048392424826,1.,0.123018905621083));
#32931=CARTESIAN_POINT('Ctrl Pts',(2.09625292867756,1.,0.120570567965129));
#32932=CARTESIAN_POINT('Ctrl Pts',(2.10201512132945,1.,0.118079107988368));
#32933=CARTESIAN_POINT('Ctrl Pts',(2.10777050261359,1.,0.11554495768794));
#32934=CARTESIAN_POINT('Ctrl Pts',(2.11351924490335,1.,0.112968534419746));
#32935=CARTESIAN_POINT('Ctrl Pts',(2.11926155590849,1.,0.11035023613502));
#32936=CARTESIAN_POINT('Ctrl Pts',(2.12499752306927,1.,0.107690435231068));
#32937=CARTESIAN_POINT('Ctrl Pts',(2.1307270488718,1.,0.104989479152703));
#32938=CARTESIAN_POINT('Ctrl Pts',(2.13644992667052,1.,0.102247700556063));
#32939=CARTESIAN_POINT('Ctrl Pts',(2.14216588395974,1.,0.0994654261990741));
#32940=CARTESIAN_POINT('Ctrl Pts',(2.14787463531864,1.,0.0966429852305688));
#32941=CARTESIAN_POINT('Ctrl Pts',(2.15357593978377,1.,0.0937807218868344));
#32942=CARTESIAN_POINT('Ctrl Pts',(2.15926961544808,1.,0.0908789888108265));
#32943=CARTESIAN_POINT('Ctrl Pts',(2.16495552645275,1.,0.0879381291387821));
#32944=CARTESIAN_POINT('Ctrl Pts',(2.17063357871031,1.,0.0849584620835642));
#32945=CARTESIAN_POINT('Ctrl Pts',(2.1763037121106,1.,0.0819402680871938));
#32946=CARTESIAN_POINT('Ctrl Pts',(2.18196589448304,1.,0.0788837727683226));
#32947=CARTESIAN_POINT('Ctrl Pts',(2.1876201139874,1.,0.075789146583341));
#32948=CARTESIAN_POINT('Ctrl Pts',(2.19213712012956,1.,0.0732830357304275));
#32949=CARTESIAN_POINT('Ctrl Pts',(2.19552129483562,1.,0.0713863779524626));
#32950=CARTESIAN_POINT('Ctrl Pts',(2.19777582085261,1.,0.0701143536324925));
#32951=CARTESIAN_POINT('Ctrl Pts',(2.19890268624765,1.,0.0694764450219582));
#32952=CARTESIAN_POINT('',(1.74236521665491,0.,0.163289472382896));
#32953=CARTESIAN_POINT('Origin',(0.,1.,0.));
#32954=CARTESIAN_POINT('Origin',(0.,1.,0.));
#32955=CARTESIAN_POINT('Origin',(0.,0.,0.));
#32956=CARTESIAN_POINT('',(0.,0.,0.));
#32957=CARTESIAN_POINT('Origin',(0.,0.,0.));
#32958=CARTESIAN_POINT('',(-0.32,0.16,3.91886975727153E-17));
#32959=CARTESIAN_POINT('Origin',(0.,0.16,0.));
#32960=CARTESIAN_POINT('',(-0.32,0.,3.91886975727153E-17));
#32961=CARTESIAN_POINT('',(-0.32,0.,3.91886975727153E-17));
#32962=CARTESIAN_POINT('Origin',(0.,0.,0.));
#32963=CARTESIAN_POINT('Origin',(0.,0.,0.));
#32964=CARTESIAN_POINT('',(-0.6,0.16,7.34788079488412E-17));
#32965=CARTESIAN_POINT('Origin',(0.,0.16,0.));
#32966=CARTESIAN_POINT('',(-0.6,0.,7.34788079488412E-17));
#32967=CARTESIAN_POINT('',(-0.6,0.,7.34788079488412E-17));
#32968=CARTESIAN_POINT('Origin',(0.,0.,0.));
#32969=CARTESIAN_POINT('Origin',(0.,0.16,0.));
#32970=CARTESIAN_POINT('Origin',(0.,0.,0.));
#32971=CARTESIAN_POINT('',(0.,0.,0.));
#32972=CARTESIAN_POINT('Origin',(0.45,0.6,0.));
#32973=CARTESIAN_POINT('',(-0.45,0.6,-5.51091059616309E-17));
#32974=CARTESIAN_POINT('Origin',(0.,0.6,0.));
#32975=CARTESIAN_POINT('Origin',(0.,0.575,0.));
#32976=CARTESIAN_POINT('',(-0.5,0.55,-6.12323399573677E-17));
#32977=CARTESIAN_POINT('Origin',(0.,0.55,0.));
#32978=CARTESIAN_POINT('',(-0.475,0.575,-5.81707229594993E-17));
#32979=CARTESIAN_POINT('Origin',(0.,0.29,0.));
#32980=CARTESIAN_POINT('',(-0.5,0.0299999999999998,-6.12323399573677E-17));
#32981=CARTESIAN_POINT('Origin',(0.,0.0299999999999998,0.));
#32982=CARTESIAN_POINT('',(-0.5,0.29,-6.12323399573677E-17));
#32983=CARTESIAN_POINT('Origin',(0.,0.0150000000000001,0.));
#32984=CARTESIAN_POINT('',(-0.47,7.11236625150491E-17,-5.75583995599256E-17));
#32985=CARTESIAN_POINT('Origin',(0.,0.,0.));
#32986=CARTESIAN_POINT('',(-0.485,0.0150000000000001,-5.93953697586466E-17));
#32987=CARTESIAN_POINT('Origin',(0.32,0.,0.));
#32988=CARTESIAN_POINT('',(-0.32,-6.93889390390723E-18,-3.91886975727153E-17));
#32989=CARTESIAN_POINT('Origin',(0.,0.,0.));
#32990=CARTESIAN_POINT('Origin',(0.,-0.02,0.));
#32991=CARTESIAN_POINT('',(-0.2942,-0.0515999999999999,3.60291088309151E-17));
#32992=CARTESIAN_POINT('Origin',(0.,-0.0515999999999999,0.));
#32993=CARTESIAN_POINT('',(-0.31,-0.02,-3.7964050773568E-17));
#32994=CARTESIAN_POINT('Origin',(0.,-1.24,0.));
#32995=CARTESIAN_POINT('',(-0.2942,-2.4458,3.60291088309151E-17));
#32996=CARTESIAN_POINT('Origin',(0.,-2.4458,0.));
#32997=CARTESIAN_POINT('',(-0.2942,-1.24,-3.60291088309151E-17));
#32998=CARTESIAN_POINT('Origin',(0.,-2.47,0.));
#32999=CARTESIAN_POINT('',(-0.24,-2.5,-2.93915231795365E-17));
#33000=CARTESIAN_POINT('Origin',(0.,-2.5,0.));
#33001=CARTESIAN_POINT('',(-0.27,-2.47,-3.30654635769785E-17));
#33002=CARTESIAN_POINT('Origin',(0.,-2.5,0.));
#33003=CARTESIAN_POINT('Origin',(0.144337567297406,-0.6,-0.25));
#33004=CARTESIAN_POINT('',(0.288675134594813,-0.6,0.));
#33005=CARTESIAN_POINT('',(0.144337567297406,-0.6,-0.25));
#33006=CARTESIAN_POINT('',(0.288675134594813,-0.6,0.));
#33007=CARTESIAN_POINT('',(0.144337567297406,-0.96,-0.25));
#33008=CARTESIAN_POINT('',(0.144337567297406,-0.6,-0.25));
#33009=CARTESIAN_POINT('',(0.288675134594813,-0.96,0.));
#33010=CARTESIAN_POINT('',(0.288675134594813,-0.96,0.));
#33011=CARTESIAN_POINT('',(0.288675134594813,-0.6,0.));
#33012=CARTESIAN_POINT('Origin',(-0.144337567297406,-0.6,-0.25));
#33013=CARTESIAN_POINT('',(-0.144337567297406,-0.6,-0.25));
#33014=CARTESIAN_POINT('',(0.144337567297406,-0.6,-0.25));
#33015=CARTESIAN_POINT('',(-0.144337567297406,-0.96,-0.25));
#33016=CARTESIAN_POINT('',(-0.144337567297406,-0.6,-0.25));
#33017=CARTESIAN_POINT('',(0.144337567297406,-0.96,-0.25));
#33018=CARTESIAN_POINT('Origin',(-0.288675134594813,-0.6,-8.32667268468867E-17));
#33019=CARTESIAN_POINT('',(-0.288675134594813,-0.6,-3.53525079574969E-17));
#33020=CARTESIAN_POINT('',(-0.144337567297406,-0.6,-0.25));
#33021=CARTESIAN_POINT('',(-0.288675134594813,-0.96,-5.55111512312578E-17));
#33022=CARTESIAN_POINT('',(-0.288675134594813,-0.6,-3.53525079574969E-17));
#33023=CARTESIAN_POINT('',(-0.144337567297406,-0.96,-0.25));
#33024=CARTESIAN_POINT('Origin',(-0.144337567297407,-0.6,0.25));
#33025=CARTESIAN_POINT('',(-0.144337567297407,-0.6,0.25));
#33026=CARTESIAN_POINT('',(-0.288675134594813,-0.6,-3.53525079574969E-17));
#33027=CARTESIAN_POINT('',(-0.144337567297407,-0.96,0.25));
#33028=CARTESIAN_POINT('',(-0.144337567297407,-0.6,0.25));
#33029=CARTESIAN_POINT('',(-0.288675134594813,-0.96,-3.53525079574969E-17));
#33030=CARTESIAN_POINT('Origin',(0.144337567297406,-0.6,0.25));
#33031=CARTESIAN_POINT('',(0.144337567297406,-0.6,0.25));
#33032=CARTESIAN_POINT('',(-0.144337567297407,-0.6,0.25));
#33033=CARTESIAN_POINT('',(0.144337567297406,-0.96,0.25));
#33034=CARTESIAN_POINT('',(0.144337567297406,-0.6,0.25));
#33035=CARTESIAN_POINT('',(-0.144337567297407,-0.96,0.25));
#33036=CARTESIAN_POINT('Origin',(0.288675134594813,-0.6,0.));
#33037=CARTESIAN_POINT('',(0.144337567297406,-0.6,0.25));
#33038=CARTESIAN_POINT('',(0.144337567297406,-0.96,0.25));
#33039=CARTESIAN_POINT('Origin',(0.,-0.6,0.));
#33040=CARTESIAN_POINT('Origin',(0.,-0.96,0.));
#33041=CARTESIAN_POINT('',(0.,0.,0.));
#33042=CARTESIAN_POINT('Origin',(0.3,0.4,0.));
#33043=CARTESIAN_POINT('',(-0.3,0.4,-3.67394039744206E-17));
#33044=CARTESIAN_POINT('Origin',(0.,0.4,0.));
#33045=CARTESIAN_POINT('Origin',(0.,0.375,0.));
#33046=CARTESIAN_POINT('',(-0.35,0.35,-4.28626379701573E-17));
#33047=CARTESIAN_POINT('Origin',(0.,0.35,0.));
#33048=CARTESIAN_POINT('',(-0.325,0.375,-3.9801020972289E-17));
#33049=CARTESIAN_POINT('Origin',(0.,0.19,0.));
#33050=CARTESIAN_POINT('',(-0.35,0.03,-4.28626379701574E-17));
#33051=CARTESIAN_POINT('Origin',(0.,0.03,0.));
#33052=CARTESIAN_POINT('',(-0.35,0.19,-4.28626379701574E-17));
#33053=CARTESIAN_POINT('Origin',(0.,0.0149999999999999,0.));
#33054=CARTESIAN_POINT('',(-0.32,-3.29597460435593E-17,-3.91886975727153E-17));
#33055=CARTESIAN_POINT('Origin',(0.,0.,0.));
#33056=CARTESIAN_POINT('',(-0.335,0.0149999999999999,-4.10256677714363E-17));
#33057=CARTESIAN_POINT('Origin',(0.22,0.,0.));
#33058=CARTESIAN_POINT('',(-0.22,-6.93889390390723E-18,-2.69422295812418E-17));
#33059=CARTESIAN_POINT('Origin',(0.,0.,0.));
#33060=CARTESIAN_POINT('Origin',(0.,-0.02,0.));
#33061=CARTESIAN_POINT('',(-0.1954,-0.0492,2.39295984553393E-17));
#33062=CARTESIAN_POINT('Origin',(0.,-0.0492,0.));
#33063=CARTESIAN_POINT('',(-0.21,-0.02,-2.57175827820944E-17));
#33064=CARTESIAN_POINT('Origin',(0.,-0.8,0.));
#33065=CARTESIAN_POINT('',(-0.1954,-1.5646,2.39295984553393E-17));
#33066=CARTESIAN_POINT('Origin',(0.,-1.5646,0.));
#33067=CARTESIAN_POINT('',(-0.1954,-0.8,-2.39295984553393E-17));
#33068=CARTESIAN_POINT('Origin',(0.,-1.58,0.));
#33069=CARTESIAN_POINT('',(-0.16,-1.6,-1.95943487863577E-17));
#33070=CARTESIAN_POINT('Origin',(0.,-1.6,0.));
#33071=CARTESIAN_POINT('',(-0.18,-1.58,-2.20436423846524E-17));
#33072=CARTESIAN_POINT('Origin',(0.,-1.6,0.));
#33073=CARTESIAN_POINT('Origin',(0.0866025403784439,-0.4,-0.15));
#33074=CARTESIAN_POINT('',(0.173205080756888,-0.4,0.));
#33075=CARTESIAN_POINT('',(0.0866025403784439,-0.4,-0.15));
#33076=CARTESIAN_POINT('',(0.173205080756888,-0.4,0.));
#33077=CARTESIAN_POINT('',(0.0866025403784439,-0.64,-0.15));
#33078=CARTESIAN_POINT('',(0.0866025403784439,-0.4,-0.15));
#33079=CARTESIAN_POINT('',(0.173205080756888,-0.64,0.));
#33080=CARTESIAN_POINT('',(0.173205080756888,-0.64,0.));
#33081=CARTESIAN_POINT('',(0.173205080756888,-0.4,0.));
#33082=CARTESIAN_POINT('Origin',(-0.0866025403784438,-0.4,-0.15));
#33083=CARTESIAN_POINT('',(-0.0866025403784438,-0.4,-0.15));
#33084=CARTESIAN_POINT('',(0.0866025403784439,-0.4,-0.15));
#33085=CARTESIAN_POINT('',(-0.0866025403784438,-0.64,-0.15));
#33086=CARTESIAN_POINT('',(-0.0866025403784438,-0.4,-0.15));
#33087=CARTESIAN_POINT('',(0.0866025403784439,-0.64,-0.15));
#33088=CARTESIAN_POINT('Origin',(-0.173205080756888,-0.4,-2.77555756156289E-17));
#33089=CARTESIAN_POINT('',(-0.173205080756888,-0.4,-2.12115047744981E-17));
#33090=CARTESIAN_POINT('',(-0.0866025403784438,-0.4,-0.15));
#33091=CARTESIAN_POINT('',(-0.173205080756888,-0.64,-2.77555756156289E-17));
#33092=CARTESIAN_POINT('',(-0.173205080756888,-0.4,-2.12115047744981E-17));
#33093=CARTESIAN_POINT('',(-0.0866025403784438,-0.64,-0.15));
#33094=CARTESIAN_POINT('Origin',(-0.0866025403784439,-0.4,0.15));
#33095=CARTESIAN_POINT('',(-0.0866025403784439,-0.4,0.15));
#33096=CARTESIAN_POINT('',(-0.173205080756888,-0.4,-2.12115047744981E-17));
#33097=CARTESIAN_POINT('',(-0.0866025403784439,-0.64,0.15));
#33098=CARTESIAN_POINT('',(-0.0866025403784439,-0.4,0.15));
#33099=CARTESIAN_POINT('',(-0.173205080756888,-0.64,-2.12115047744981E-17));
#33100=CARTESIAN_POINT('Origin',(0.0866025403784439,-0.4,0.15));
#33101=CARTESIAN_POINT('',(0.0866025403784439,-0.4,0.15));
#33102=CARTESIAN_POINT('',(-0.0866025403784439,-0.4,0.15));
#33103=CARTESIAN_POINT('',(0.0866025403784439,-0.64,0.15));
#33104=CARTESIAN_POINT('',(0.0866025403784439,-0.4,0.15));
#33105=CARTESIAN_POINT('',(-0.0866025403784439,-0.64,0.15));
#33106=CARTESIAN_POINT('Origin',(0.173205080756888,-0.4,0.));
#33107=CARTESIAN_POINT('',(0.0866025403784439,-0.4,0.15));
#33108=CARTESIAN_POINT('',(0.0866025403784439,-0.64,0.15));
#33109=CARTESIAN_POINT('Origin',(0.,-0.4,-2.77555756156289E-17));
#33110=CARTESIAN_POINT('Origin',(0.,-0.64,-2.77555756156289E-17));
#33111=CARTESIAN_POINT('',(0.,0.,0.));
#33112=CARTESIAN_POINT('',(0.,0.,0.));
#33113=CARTESIAN_POINT('',(0.,0.,0.));
#33114=CARTESIAN_POINT('',(0.,0.,0.));
#33115=CARTESIAN_POINT('',(0.,0.,0.));
#33116=CARTESIAN_POINT('',(0.,0.,0.));
#33117=CARTESIAN_POINT('',(0.,0.,0.));
#33118=CARTESIAN_POINT('',(0.,0.,0.));
#33119=CARTESIAN_POINT('',(0.,0.,0.));
#33120=CARTESIAN_POINT('',(0.,0.,0.));
#33121=CARTESIAN_POINT('',(0.,0.,0.));
#33122=CARTESIAN_POINT('',(0.,0.,0.));
#33123=CARTESIAN_POINT('',(0.,0.,0.));
#33124=CARTESIAN_POINT('',(0.,0.,0.));
#33125=CARTESIAN_POINT('',(0.,0.,0.));
#33126=CARTESIAN_POINT('',(0.,0.,0.));
#33127=CARTESIAN_POINT('',(5.5,0.,1.));
#33128=CARTESIAN_POINT('',(5.5,-1.6,1.5));
#33129=CARTESIAN_POINT('',(5.5,1.6,1.5));
#33130=CARTESIAN_POINT('',(6.7,0.,2.));
#33131=CARTESIAN_POINT('',(6.7,0.,12.2));
#33132=CARTESIAN_POINT('',(2.4,-1.6,15.6));
#33133=CARTESIAN_POINT('',(2.4,1.6,15.6));
#33134=CARTESIAN_POINT('',(2.4,-1.6,25.6));
#33135=CARTESIAN_POINT('',(2.4,1.6,25.6));
#33136=CARTESIAN_POINT('',(6.7,0.,3.75));
#33137=CARTESIAN_POINT('',(-6.05,-3.,1.8));
#33138=CARTESIAN_POINT('',(-0.45,-3.,1.8));
#33139=CARTESIAN_POINT('',(-3.25,-3.,20.));
#33140=CARTESIAN_POINT('',(-1.83578643762691,-4.,21.4142135623731));
#33141=CARTESIAN_POINT('',(-4.6642135623731,-4.,21.4142135623731));
#33142=CARTESIAN_POINT('',(-4.6642135623731,-4.,18.5857864376269));
#33143=CARTESIAN_POINT('',(-1.83578643762691,-4.,18.5857864376269));
#33144=CARTESIAN_POINT('',(-1.83578643762691,-2.,21.4142135623731));
#33145=CARTESIAN_POINT('',(-4.6642135623731,-2.,21.4142135623731));
#33146=CARTESIAN_POINT('',(-4.6642135623731,-2.,18.5857864376269));
#33147=CARTESIAN_POINT('',(-1.83578643762691,-2.,18.5857864376269));
#33148=CARTESIAN_POINT('',(-6.05,3.,1.8));
#33149=CARTESIAN_POINT('',(-0.45,3.,1.8));
#33150=CARTESIAN_POINT('',(-3.25,3.,20.));
#33151=CARTESIAN_POINT('',(-1.83578643762691,2.,21.4142135623731));
#33152=CARTESIAN_POINT('',(-4.6642135623731,2.,21.4142135623731));
#33153=CARTESIAN_POINT('',(-4.6642135623731,2.,18.5857864376269));
#33154=CARTESIAN_POINT('',(-1.83578643762691,2.,18.5857864376269));
#33155=CARTESIAN_POINT('',(-1.83578643762691,4.,21.4142135623731));
#33156=CARTESIAN_POINT('',(-4.6642135623731,4.,21.4142135623731));
#33157=CARTESIAN_POINT('',(-4.6642135623731,4.,18.5857864376269));
#33158=CARTESIAN_POINT('',(-1.83578643762691,4.,18.5857864376269));
#33159=CARTESIAN_POINT('',(0.,0.,0.));
#33160=CARTESIAN_POINT('',(0.,0.,0.));
#33161=CARTESIAN_POINT('',(0.,0.,0.));
#33162=CARTESIAN_POINT('',(0.,0.,0.));
#33163=CARTESIAN_POINT('',(0.,0.,0.));
#33164=CARTESIAN_POINT('',(0.,0.,0.));
#33165=CARTESIAN_POINT('',(0.,0.,0.));
#33166=CARTESIAN_POINT('',(0.,0.,0.));
#33167=CARTESIAN_POINT('',(0.,0.,0.));
#33168=CARTESIAN_POINT('',(0.,0.,0.));
#33169=CARTESIAN_POINT('',(0.,0.,0.));
#33170=CARTESIAN_POINT('',(-3.25,0.,20.));
#33171=CARTESIAN_POINT('',(-3.25,8.4,29.));
#33172=CARTESIAN_POINT('',(-3.25,8.56,29.));
#33173=CARTESIAN_POINT('',(-3.25,-5.7,20.));
#33174=CARTESIAN_POINT('',(-3.25,7.7,20.));
#33175=CARTESIAN_POINT('',(0.,0.,0.));
#33176=CARTESIAN_POINT('',(0.,0.,0.));
#33177=CARTESIAN_POINT('Origin',(-3.25,6.8,29.));
#33178=CARTESIAN_POINT('',(-3.655,8.37,29.));
#33179=CARTESIAN_POINT('Origin',(-3.25,8.37,29.));
#33180=CARTESIAN_POINT('',(-3.655,6.8,29.));
#33181=CARTESIAN_POINT('',(-3.655,6.8,29.));
#33182=CARTESIAN_POINT('Origin',(-3.25,6.8,29.));
#33183=CARTESIAN_POINT('Origin',(-3.25,6.8,29.));
#33184=CARTESIAN_POINT('',(-4.15,8.37,29.));
#33185=CARTESIAN_POINT('Origin',(-3.25,8.37,29.));
#33186=CARTESIAN_POINT('',(-4.15,6.8,29.));
#33187=CARTESIAN_POINT('',(-4.15,6.8,29.));
#33188=CARTESIAN_POINT('Origin',(-3.25,6.8,29.));
#33189=CARTESIAN_POINT('Origin',(-3.25,8.37,29.));
#33190=CARTESIAN_POINT('Origin',(-3.25,6.8,29.));
#33191=CARTESIAN_POINT('',(0.,0.,0.));
#33192=CARTESIAN_POINT('',(0.,0.,0.));
#33193=CARTESIAN_POINT('',(0.,0.,0.));
#33194=CARTESIAN_POINT('',(0.,0.,0.));
#33195=CARTESIAN_POINT('',(0.,0.,0.));
#33196=UNCERTAINTY_MEASURE_WITH_UNIT(LENGTH_MEASURE(0.001),#33300,
'DISTANCE_ACCURACY_VALUE',
'Maximum model space distance between geometric entities at asserted c
onnectivities');
#33197=UNCERTAINTY_MEASURE_WITH_UNIT(LENGTH_MEASURE(0.001),#33300,
'DISTANCE_ACCURACY_VALUE',
'Maximum model space distance between geometric entities at asserted c
onnectivities');
#33198=UNCERTAINTY_MEASURE_WITH_UNIT(LENGTH_MEASURE(0.001),#33300,
'DISTANCE_ACCURACY_VALUE',
'Maximum model space distance between geometric entities at asserted c
onnectivities');
#33199=UNCERTAINTY_MEASURE_WITH_UNIT(LENGTH_MEASURE(0.001),#33300,
'DISTANCE_ACCURACY_VALUE',
'Maximum model space distance between geometric entities at asserted c
onnectivities');
#33200=UNCERTAINTY_MEASURE_WITH_UNIT(LENGTH_MEASURE(0.001),#33300,
'DISTANCE_ACCURACY_VALUE',
'Maximum model space distance between geometric entities at asserted c
onnectivities');
#33201=UNCERTAINTY_MEASURE_WITH_UNIT(LENGTH_MEASURE(0.001),#33300,
'DISTANCE_ACCURACY_VALUE',
'Maximum model space distance between geometric entities at asserted c
onnectivities');
#33202=UNCERTAINTY_MEASURE_WITH_UNIT(LENGTH_MEASURE(0.001),#33300,
'DISTANCE_ACCURACY_VALUE',
'Maximum model space distance between geometric entities at asserted c
onnectivities');
#33203=UNCERTAINTY_MEASURE_WITH_UNIT(LENGTH_MEASURE(0.001),#33300,
'DISTANCE_ACCURACY_VALUE',
'Maximum model space distance between geometric entities at asserted c
onnectivities');
#33204=UNCERTAINTY_MEASURE_WITH_UNIT(LENGTH_MEASURE(0.001),#33300,
'DISTANCE_ACCURACY_VALUE',
'Maximum model space distance between geometric entities at asserted c
onnectivities');
#33205=UNCERTAINTY_MEASURE_WITH_UNIT(LENGTH_MEASURE(0.001),#33300,
'DISTANCE_ACCURACY_VALUE',
'Maximum model space distance between geometric entities at asserted c
onnectivities');
#33206=UNCERTAINTY_MEASURE_WITH_UNIT(LENGTH_MEASURE(0.001),#33300,
'DISTANCE_ACCURACY_VALUE',
'Maximum model space distance between geometric entities at asserted c
onnectivities');
#33207=UNCERTAINTY_MEASURE_WITH_UNIT(LENGTH_MEASURE(0.001),#33300,
'DISTANCE_ACCURACY_VALUE',
'Maximum model space distance between geometric entities at asserted c
onnectivities');
#33208=UNCERTAINTY_MEASURE_WITH_UNIT(LENGTH_MEASURE(0.001),#33300,
'DISTANCE_ACCURACY_VALUE',
'Maximum model space distance between geometric entities at asserted c
onnectivities');
#33209=UNCERTAINTY_MEASURE_WITH_UNIT(LENGTH_MEASURE(0.001),#33300,
'DISTANCE_ACCURACY_VALUE',
'Maximum model space distance between geometric entities at asserted c
onnectivities');
#33210=UNCERTAINTY_MEASURE_WITH_UNIT(LENGTH_MEASURE(0.001),#33300,
'DISTANCE_ACCURACY_VALUE',
'Maximum model space distance between geometric entities at asserted c
onnectivities');
#33211=UNCERTAINTY_MEASURE_WITH_UNIT(LENGTH_MEASURE(0.001),#33300,
'DISTANCE_ACCURACY_VALUE',
'Maximum model space distance between geometric entities at asserted c
onnectivities');
#33212=UNCERTAINTY_MEASURE_WITH_UNIT(LENGTH_MEASURE(0.001),#33300,
'DISTANCE_ACCURACY_VALUE',
'Maximum model space distance between geometric entities at asserted c
onnectivities');
#33213=UNCERTAINTY_MEASURE_WITH_UNIT(LENGTH_MEASURE(0.001),#33300,
'DISTANCE_ACCURACY_VALUE',
'Maximum model space distance between geometric entities at asserted c
onnectivities');
#33214=UNCERTAINTY_MEASURE_WITH_UNIT(LENGTH_MEASURE(0.001),#33300,
'DISTANCE_ACCURACY_VALUE',
'Maximum model space distance between geometric entities at asserted c
onnectivities');
#33215=UNCERTAINTY_MEASURE_WITH_UNIT(LENGTH_MEASURE(0.001),#33300,
'DISTANCE_ACCURACY_VALUE',
'Maximum model space distance between geometric entities at asserted c
onnectivities');
#33216=UNCERTAINTY_MEASURE_WITH_UNIT(LENGTH_MEASURE(0.001),#33300,
'DISTANCE_ACCURACY_VALUE',
'Maximum model space distance between geometric entities at asserted c
onnectivities');
#33217=UNCERTAINTY_MEASURE_WITH_UNIT(LENGTH_MEASURE(0.001),#33300,
'DISTANCE_ACCURACY_VALUE',
'Maximum model space distance between geometric entities at asserted c
onnectivities');
#33218=UNCERTAINTY_MEASURE_WITH_UNIT(LENGTH_MEASURE(0.001),#33300,
'DISTANCE_ACCURACY_VALUE',
'Maximum model space distance between geometric entities at asserted c
onnectivities');
#33219=UNCERTAINTY_MEASURE_WITH_UNIT(LENGTH_MEASURE(0.001),#33300,
'DISTANCE_ACCURACY_VALUE',
'Maximum model space distance between geometric entities at asserted c
onnectivities');
#33220=UNCERTAINTY_MEASURE_WITH_UNIT(LENGTH_MEASURE(0.001),#33300,
'DISTANCE_ACCURACY_VALUE',
'Maximum model space distance between geometric entities at asserted c
onnectivities');
#33221=UNCERTAINTY_MEASURE_WITH_UNIT(LENGTH_MEASURE(0.001),#33300,
'DISTANCE_ACCURACY_VALUE',
'Maximum model space distance between geometric entities at asserted c
onnectivities');
#33222=UNCERTAINTY_MEASURE_WITH_UNIT(LENGTH_MEASURE(0.001),#33300,
'DISTANCE_ACCURACY_VALUE',
'Maximum model space distance between geometric entities at asserted c
onnectivities');
#33223=UNCERTAINTY_MEASURE_WITH_UNIT(LENGTH_MEASURE(0.001),#33300,
'DISTANCE_ACCURACY_VALUE',
'Maximum model space distance between geometric entities at asserted c
onnectivities');
#33224=UNCERTAINTY_MEASURE_WITH_UNIT(LENGTH_MEASURE(0.001),#33300,
'DISTANCE_ACCURACY_VALUE',
'Maximum model space distance between geometric entities at asserted c
onnectivities');
#33225=UNCERTAINTY_MEASURE_WITH_UNIT(LENGTH_MEASURE(0.001),#33300,
'DISTANCE_ACCURACY_VALUE',
'Maximum model space distance between geometric entities at asserted c
onnectivities');
#33226=UNCERTAINTY_MEASURE_WITH_UNIT(LENGTH_MEASURE(0.001),#33300,
'DISTANCE_ACCURACY_VALUE',
'Maximum model space distance between geometric entities at asserted c
onnectivities');
#33227=UNCERTAINTY_MEASURE_WITH_UNIT(LENGTH_MEASURE(0.001),#33300,
'DISTANCE_ACCURACY_VALUE',
'Maximum model space distance between geometric entities at asserted c
onnectivities');
#33228=UNCERTAINTY_MEASURE_WITH_UNIT(LENGTH_MEASURE(0.001),#33300,
'DISTANCE_ACCURACY_VALUE',
'Maximum model space distance between geometric entities at asserted c
onnectivities');
#33229=UNCERTAINTY_MEASURE_WITH_UNIT(LENGTH_MEASURE(0.001),#33300,
'DISTANCE_ACCURACY_VALUE',
'Maximum model space distance between geometric entities at asserted c
onnectivities');
#33230=UNCERTAINTY_MEASURE_WITH_UNIT(LENGTH_MEASURE(0.001),#33300,
'DISTANCE_ACCURACY_VALUE',
'Maximum model space distance between geometric entities at asserted c
onnectivities');
#33231=UNCERTAINTY_MEASURE_WITH_UNIT(LENGTH_MEASURE(0.001),#33300,
'DISTANCE_ACCURACY_VALUE',
'Maximum model space distance between geometric entities at asserted c
onnectivities');
#33232=UNCERTAINTY_MEASURE_WITH_UNIT(LENGTH_MEASURE(0.001),#33300,
'DISTANCE_ACCURACY_VALUE',
'Maximum model space distance between geometric entities at asserted c
onnectivities');
#33233=UNCERTAINTY_MEASURE_WITH_UNIT(LENGTH_MEASURE(0.001),#33300,
'DISTANCE_ACCURACY_VALUE',
'Maximum model space distance between geometric entities at asserted c
onnectivities');
#33234=UNCERTAINTY_MEASURE_WITH_UNIT(LENGTH_MEASURE(0.001),#33300,
'DISTANCE_ACCURACY_VALUE',
'Maximum model space distance between geometric entities at asserted c
onnectivities');
#33235=UNCERTAINTY_MEASURE_WITH_UNIT(LENGTH_MEASURE(0.001),#33300,
'DISTANCE_ACCURACY_VALUE',
'Maximum model space distance between geometric entities at asserted c
onnectivities');
#33236=UNCERTAINTY_MEASURE_WITH_UNIT(LENGTH_MEASURE(0.001),#33300,
'DISTANCE_ACCURACY_VALUE',
'Maximum model space distance between geometric entities at asserted c
onnectivities');
#33237=UNCERTAINTY_MEASURE_WITH_UNIT(LENGTH_MEASURE(0.001),#33300,
'DISTANCE_ACCURACY_VALUE',
'Maximum model space distance between geometric entities at asserted c
onnectivities');
#33238=UNCERTAINTY_MEASURE_WITH_UNIT(LENGTH_MEASURE(0.001),#33300,
'DISTANCE_ACCURACY_VALUE',
'Maximum model space distance between geometric entities at asserted c
onnectivities');
#33239=UNCERTAINTY_MEASURE_WITH_UNIT(LENGTH_MEASURE(0.001),#33300,
'DISTANCE_ACCURACY_VALUE',
'Maximum model space distance between geometric entities at asserted c
onnectivities');
#33240=UNCERTAINTY_MEASURE_WITH_UNIT(LENGTH_MEASURE(0.001),#33300,
'DISTANCE_ACCURACY_VALUE',
'Maximum model space distance between geometric entities at asserted c
onnectivities');
#33241=UNCERTAINTY_MEASURE_WITH_UNIT(LENGTH_MEASURE(0.001),#33300,
'DISTANCE_ACCURACY_VALUE',
'Maximum model space distance between geometric entities at asserted c
onnectivities');
#33242=UNCERTAINTY_MEASURE_WITH_UNIT(LENGTH_MEASURE(0.001),#33300,
'DISTANCE_ACCURACY_VALUE',
'Maximum model space distance between geometric entities at asserted c
onnectivities');
#33243=UNCERTAINTY_MEASURE_WITH_UNIT(LENGTH_MEASURE(0.001),#33300,
'DISTANCE_ACCURACY_VALUE',
'Maximum model space distance between geometric entities at asserted c
onnectivities');
#33244=UNCERTAINTY_MEASURE_WITH_UNIT(LENGTH_MEASURE(0.001),#33300,
'DISTANCE_ACCURACY_VALUE',
'Maximum model space distance between geometric entities at asserted c
onnectivities');
#33245=UNCERTAINTY_MEASURE_WITH_UNIT(LENGTH_MEASURE(0.001),#33300,
'DISTANCE_ACCURACY_VALUE',
'Maximum model space distance between geometric entities at asserted c
onnectivities');
#33246=UNCERTAINTY_MEASURE_WITH_UNIT(LENGTH_MEASURE(0.001),#33300,
'DISTANCE_ACCURACY_VALUE',
'Maximum model space distance between geometric entities at asserted c
onnectivities');
#33247=UNCERTAINTY_MEASURE_WITH_UNIT(LENGTH_MEASURE(0.001),#33300,
'DISTANCE_ACCURACY_VALUE',
'Maximum model space distance between geometric entities at asserted c
onnectivities');
#33248=(
GEOMETRIC_REPRESENTATION_CONTEXT(3)
GLOBAL_UNCERTAINTY_ASSIGNED_CONTEXT((#33196))
GLOBAL_UNIT_ASSIGNED_CONTEXT((#33300,#33302,#33303))
REPRESENTATION_CONTEXT('','3D')
);
#33249=(
GEOMETRIC_REPRESENTATION_CONTEXT(3)
GLOBAL_UNCERTAINTY_ASSIGNED_CONTEXT((#33197))
GLOBAL_UNIT_ASSIGNED_CONTEXT((#33300,#33302,#33303))
REPRESENTATION_CONTEXT('','3D')
);
#33250=(
GEOMETRIC_REPRESENTATION_CONTEXT(3)
GLOBAL_UNCERTAINTY_ASSIGNED_CONTEXT((#33198))
GLOBAL_UNIT_ASSIGNED_CONTEXT((#33300,#33302,#33303))
REPRESENTATION_CONTEXT('','3D')
);
#33251=(
GEOMETRIC_REPRESENTATION_CONTEXT(3)
GLOBAL_UNCERTAINTY_ASSIGNED_CONTEXT((#33199))
GLOBAL_UNIT_ASSIGNED_CONTEXT((#33300,#33302,#33303))
REPRESENTATION_CONTEXT('','3D')
);
#33252=(
GEOMETRIC_REPRESENTATION_CONTEXT(3)
GLOBAL_UNCERTAINTY_ASSIGNED_CONTEXT((#33200))
GLOBAL_UNIT_ASSIGNED_CONTEXT((#33300,#33302,#33303))
REPRESENTATION_CONTEXT('','3D')
);
#33253=(
GEOMETRIC_REPRESENTATION_CONTEXT(3)
GLOBAL_UNCERTAINTY_ASSIGNED_CONTEXT((#33201))
GLOBAL_UNIT_ASSIGNED_CONTEXT((#33300,#33302,#33303))
REPRESENTATION_CONTEXT('','3D')
);
#33254=(
GEOMETRIC_REPRESENTATION_CONTEXT(3)
GLOBAL_UNCERTAINTY_ASSIGNED_CONTEXT((#33202))
GLOBAL_UNIT_ASSIGNED_CONTEXT((#33300,#33302,#33303))
REPRESENTATION_CONTEXT('','3D')
);
#33255=(
GEOMETRIC_REPRESENTATION_CONTEXT(3)
GLOBAL_UNCERTAINTY_ASSIGNED_CONTEXT((#33203))
GLOBAL_UNIT_ASSIGNED_CONTEXT((#33300,#33302,#33303))
REPRESENTATION_CONTEXT('','3D')
);
#33256=(
GEOMETRIC_REPRESENTATION_CONTEXT(3)
GLOBAL_UNCERTAINTY_ASSIGNED_CONTEXT((#33204))
GLOBAL_UNIT_ASSIGNED_CONTEXT((#33300,#33302,#33303))
REPRESENTATION_CONTEXT('','3D')
);
#33257=(
GEOMETRIC_REPRESENTATION_CONTEXT(3)
GLOBAL_UNCERTAINTY_ASSIGNED_CONTEXT((#33205))
GLOBAL_UNIT_ASSIGNED_CONTEXT((#33300,#33302,#33303))
REPRESENTATION_CONTEXT('','3D')
);
#33258=(
GEOMETRIC_REPRESENTATION_CONTEXT(3)
GLOBAL_UNCERTAINTY_ASSIGNED_CONTEXT((#33206))
GLOBAL_UNIT_ASSIGNED_CONTEXT((#33300,#33302,#33303))
REPRESENTATION_CONTEXT('','3D')
);
#33259=(
GEOMETRIC_REPRESENTATION_CONTEXT(3)
GLOBAL_UNCERTAINTY_ASSIGNED_CONTEXT((#33207))
GLOBAL_UNIT_ASSIGNED_CONTEXT((#33300,#33302,#33303))
REPRESENTATION_CONTEXT('','3D')
);
#33260=(
GEOMETRIC_REPRESENTATION_CONTEXT(3)
GLOBAL_UNCERTAINTY_ASSIGNED_CONTEXT((#33208))
GLOBAL_UNIT_ASSIGNED_CONTEXT((#33300,#33302,#33303))
REPRESENTATION_CONTEXT('','3D')
);
#33261=(
GEOMETRIC_REPRESENTATION_CONTEXT(3)
GLOBAL_UNCERTAINTY_ASSIGNED_CONTEXT((#33209))
GLOBAL_UNIT_ASSIGNED_CONTEXT((#33300,#33302,#33303))
REPRESENTATION_CONTEXT('','3D')
);
#33262=(
GEOMETRIC_REPRESENTATION_CONTEXT(3)
GLOBAL_UNCERTAINTY_ASSIGNED_CONTEXT((#33210))
GLOBAL_UNIT_ASSIGNED_CONTEXT((#33300,#33302,#33303))
REPRESENTATION_CONTEXT('','3D')
);
#33263=(
GEOMETRIC_REPRESENTATION_CONTEXT(3)
GLOBAL_UNCERTAINTY_ASSIGNED_CONTEXT((#33211))
GLOBAL_UNIT_ASSIGNED_CONTEXT((#33300,#33302,#33303))
REPRESENTATION_CONTEXT('','3D')
);
#33264=(
GEOMETRIC_REPRESENTATION_CONTEXT(3)
GLOBAL_UNCERTAINTY_ASSIGNED_CONTEXT((#33212))
GLOBAL_UNIT_ASSIGNED_CONTEXT((#33300,#33302,#33303))
REPRESENTATION_CONTEXT('','3D')
);
#33265=(
GEOMETRIC_REPRESENTATION_CONTEXT(3)
GLOBAL_UNCERTAINTY_ASSIGNED_CONTEXT((#33213))
GLOBAL_UNIT_ASSIGNED_CONTEXT((#33300,#33302,#33303))
REPRESENTATION_CONTEXT('','3D')
);
#33266=(
GEOMETRIC_REPRESENTATION_CONTEXT(3)
GLOBAL_UNCERTAINTY_ASSIGNED_CONTEXT((#33214))
GLOBAL_UNIT_ASSIGNED_CONTEXT((#33300,#33302,#33303))
REPRESENTATION_CONTEXT('','3D')
);
#33267=(
GEOMETRIC_REPRESENTATION_CONTEXT(3)
GLOBAL_UNCERTAINTY_ASSIGNED_CONTEXT((#33215))
GLOBAL_UNIT_ASSIGNED_CONTEXT((#33300,#33302,#33303))
REPRESENTATION_CONTEXT('','3D')
);
#33268=(
GEOMETRIC_REPRESENTATION_CONTEXT(3)
GLOBAL_UNCERTAINTY_ASSIGNED_CONTEXT((#33216))
GLOBAL_UNIT_ASSIGNED_CONTEXT((#33300,#33302,#33303))
REPRESENTATION_CONTEXT('','3D')
);
#33269=(
GEOMETRIC_REPRESENTATION_CONTEXT(3)
GLOBAL_UNCERTAINTY_ASSIGNED_CONTEXT((#33217))
GLOBAL_UNIT_ASSIGNED_CONTEXT((#33300,#33302,#33303))
REPRESENTATION_CONTEXT('','3D')
);
#33270=(
GEOMETRIC_REPRESENTATION_CONTEXT(3)
GLOBAL_UNCERTAINTY_ASSIGNED_CONTEXT((#33218))
GLOBAL_UNIT_ASSIGNED_CONTEXT((#33300,#33302,#33303))
REPRESENTATION_CONTEXT('','3D')
);
#33271=(
GEOMETRIC_REPRESENTATION_CONTEXT(3)
GLOBAL_UNCERTAINTY_ASSIGNED_CONTEXT((#33219))
GLOBAL_UNIT_ASSIGNED_CONTEXT((#33300,#33302,#33303))
REPRESENTATION_CONTEXT('','3D')
);
#33272=(
GEOMETRIC_REPRESENTATION_CONTEXT(3)
GLOBAL_UNCERTAINTY_ASSIGNED_CONTEXT((#33220))
GLOBAL_UNIT_ASSIGNED_CONTEXT((#33300,#33302,#33303))
REPRESENTATION_CONTEXT('','3D')
);
#33273=(
GEOMETRIC_REPRESENTATION_CONTEXT(3)
GLOBAL_UNCERTAINTY_ASSIGNED_CONTEXT((#33221))
GLOBAL_UNIT_ASSIGNED_CONTEXT((#33300,#33302,#33303))
REPRESENTATION_CONTEXT('','3D')
);
#33274=(
GEOMETRIC_REPRESENTATION_CONTEXT(3)
GLOBAL_UNCERTAINTY_ASSIGNED_CONTEXT((#33222))
GLOBAL_UNIT_ASSIGNED_CONTEXT((#33300,#33302,#33303))
REPRESENTATION_CONTEXT('','3D')
);
#33275=(
GEOMETRIC_REPRESENTATION_CONTEXT(3)
GLOBAL_UNCERTAINTY_ASSIGNED_CONTEXT((#33223))
GLOBAL_UNIT_ASSIGNED_CONTEXT((#33300,#33302,#33303))
REPRESENTATION_CONTEXT('','3D')
);
#33276=(
GEOMETRIC_REPRESENTATION_CONTEXT(3)
GLOBAL_UNCERTAINTY_ASSIGNED_CONTEXT((#33224))
GLOBAL_UNIT_ASSIGNED_CONTEXT((#33300,#33302,#33303))
REPRESENTATION_CONTEXT('','3D')
);
#33277=(
GEOMETRIC_REPRESENTATION_CONTEXT(3)
GLOBAL_UNCERTAINTY_ASSIGNED_CONTEXT((#33225))
GLOBAL_UNIT_ASSIGNED_CONTEXT((#33300,#33302,#33303))
REPRESENTATION_CONTEXT('','3D')
);
#33278=(
GEOMETRIC_REPRESENTATION_CONTEXT(3)
GLOBAL_UNCERTAINTY_ASSIGNED_CONTEXT((#33226))
GLOBAL_UNIT_ASSIGNED_CONTEXT((#33300,#33302,#33303))
REPRESENTATION_CONTEXT('','3D')
);
#33279=(
GEOMETRIC_REPRESENTATION_CONTEXT(3)
GLOBAL_UNCERTAINTY_ASSIGNED_CONTEXT((#33227))
GLOBAL_UNIT_ASSIGNED_CONTEXT((#33300,#33302,#33303))
REPRESENTATION_CONTEXT('','3D')
);
#33280=(
GEOMETRIC_REPRESENTATION_CONTEXT(3)
GLOBAL_UNCERTAINTY_ASSIGNED_CONTEXT((#33228))
GLOBAL_UNIT_ASSIGNED_CONTEXT((#33300,#33302,#33303))
REPRESENTATION_CONTEXT('','3D')
);
#33281=(
GEOMETRIC_REPRESENTATION_CONTEXT(3)
GLOBAL_UNCERTAINTY_ASSIGNED_CONTEXT((#33229))
GLOBAL_UNIT_ASSIGNED_CONTEXT((#33300,#33302,#33303))
REPRESENTATION_CONTEXT('','3D')
);
#33282=(
GEOMETRIC_REPRESENTATION_CONTEXT(3)
GLOBAL_UNCERTAINTY_ASSIGNED_CONTEXT((#33230))
GLOBAL_UNIT_ASSIGNED_CONTEXT((#33300,#33302,#33303))
REPRESENTATION_CONTEXT('','3D')
);
#33283=(
GEOMETRIC_REPRESENTATION_CONTEXT(3)
GLOBAL_UNCERTAINTY_ASSIGNED_CONTEXT((#33231))
GLOBAL_UNIT_ASSIGNED_CONTEXT((#33300,#33302,#33303))
REPRESENTATION_CONTEXT('','3D')
);
#33284=(
GEOMETRIC_REPRESENTATION_CONTEXT(3)
GLOBAL_UNCERTAINTY_ASSIGNED_CONTEXT((#33232))
GLOBAL_UNIT_ASSIGNED_CONTEXT((#33300,#33302,#33303))
REPRESENTATION_CONTEXT('','3D')
);
#33285=(
GEOMETRIC_REPRESENTATION_CONTEXT(3)
GLOBAL_UNCERTAINTY_ASSIGNED_CONTEXT((#33233))
GLOBAL_UNIT_ASSIGNED_CONTEXT((#33300,#33302,#33303))
REPRESENTATION_CONTEXT('','3D')
);
#33286=(
GEOMETRIC_REPRESENTATION_CONTEXT(3)
GLOBAL_UNCERTAINTY_ASSIGNED_CONTEXT((#33234))
GLOBAL_UNIT_ASSIGNED_CONTEXT((#33300,#33302,#33303))
REPRESENTATION_CONTEXT('','3D')
);
#33287=(
GEOMETRIC_REPRESENTATION_CONTEXT(3)
GLOBAL_UNCERTAINTY_ASSIGNED_CONTEXT((#33235))
GLOBAL_UNIT_ASSIGNED_CONTEXT((#33300,#33302,#33303))
REPRESENTATION_CONTEXT('','3D')
);
#33288=(
GEOMETRIC_REPRESENTATION_CONTEXT(3)
GLOBAL_UNCERTAINTY_ASSIGNED_CONTEXT((#33236))
GLOBAL_UNIT_ASSIGNED_CONTEXT((#33300,#33302,#33303))
REPRESENTATION_CONTEXT('','3D')
);
#33289=(
GEOMETRIC_REPRESENTATION_CONTEXT(3)
GLOBAL_UNCERTAINTY_ASSIGNED_CONTEXT((#33237))
GLOBAL_UNIT_ASSIGNED_CONTEXT((#33300,#33302,#33303))
REPRESENTATION_CONTEXT('','3D')
);
#33290=(
GEOMETRIC_REPRESENTATION_CONTEXT(3)
GLOBAL_UNCERTAINTY_ASSIGNED_CONTEXT((#33238))
GLOBAL_UNIT_ASSIGNED_CONTEXT((#33300,#33302,#33303))
REPRESENTATION_CONTEXT('','3D')
);
#33291=(
GEOMETRIC_REPRESENTATION_CONTEXT(3)
GLOBAL_UNCERTAINTY_ASSIGNED_CONTEXT((#33239))
GLOBAL_UNIT_ASSIGNED_CONTEXT((#33300,#33302,#33303))
REPRESENTATION_CONTEXT('','3D')
);
#33292=(
GEOMETRIC_REPRESENTATION_CONTEXT(3)
GLOBAL_UNCERTAINTY_ASSIGNED_CONTEXT((#33240))
GLOBAL_UNIT_ASSIGNED_CONTEXT((#33300,#33302,#33303))
REPRESENTATION_CONTEXT('','3D')
);
#33293=(
GEOMETRIC_REPRESENTATION_CONTEXT(3)
GLOBAL_UNCERTAINTY_ASSIGNED_CONTEXT((#33241))
GLOBAL_UNIT_ASSIGNED_CONTEXT((#33300,#33302,#33303))
REPRESENTATION_CONTEXT('','3D')
);
#33294=(
GEOMETRIC_REPRESENTATION_CONTEXT(3)
GLOBAL_UNCERTAINTY_ASSIGNED_CONTEXT((#33242))
GLOBAL_UNIT_ASSIGNED_CONTEXT((#33300,#33302,#33303))
REPRESENTATION_CONTEXT('','3D')
);
#33295=(
GEOMETRIC_REPRESENTATION_CONTEXT(3)
GLOBAL_UNCERTAINTY_ASSIGNED_CONTEXT((#33243))
GLOBAL_UNIT_ASSIGNED_CONTEXT((#33300,#33302,#33303))
REPRESENTATION_CONTEXT('','3D')
);
#33296=(
GEOMETRIC_REPRESENTATION_CONTEXT(3)
GLOBAL_UNCERTAINTY_ASSIGNED_CONTEXT((#33244))
GLOBAL_UNIT_ASSIGNED_CONTEXT((#33300,#33302,#33303))
REPRESENTATION_CONTEXT('','3D')
);
#33297=(
GEOMETRIC_REPRESENTATION_CONTEXT(3)
GLOBAL_UNCERTAINTY_ASSIGNED_CONTEXT((#33245))
GLOBAL_UNIT_ASSIGNED_CONTEXT((#33300,#33302,#33303))
REPRESENTATION_CONTEXT('','3D')
);
#33298=(
GEOMETRIC_REPRESENTATION_CONTEXT(3)
GLOBAL_UNCERTAINTY_ASSIGNED_CONTEXT((#33246))
GLOBAL_UNIT_ASSIGNED_CONTEXT((#33300,#33302,#33303))
REPRESENTATION_CONTEXT('','3D')
);
#33299=(
GEOMETRIC_REPRESENTATION_CONTEXT(3)
GLOBAL_UNCERTAINTY_ASSIGNED_CONTEXT((#33247))
GLOBAL_UNIT_ASSIGNED_CONTEXT((#33300,#33302,#33303))
REPRESENTATION_CONTEXT('','3D')
);
#33300=(
LENGTH_UNIT()
NAMED_UNIT(*)
SI_UNIT(.CENTI.,.METRE.)
);
#33301=(
LENGTH_UNIT()
NAMED_UNIT(*)
SI_UNIT($,.METRE.)
);
#33302=(
NAMED_UNIT(*)
PLANE_ANGLE_UNIT()
SI_UNIT($,.RADIAN.)
);
#33303=(
NAMED_UNIT(*)
SI_UNIT($,.STERADIAN.)
SOLID_ANGLE_UNIT()
);
#33304=SHAPE_DEFINITION_REPRESENTATION(#33355,#33486);
#33305=SHAPE_DEFINITION_REPRESENTATION(#33356,#33487);
#33306=SHAPE_DEFINITION_REPRESENTATION(#33357,#33488);
#33307=SHAPE_DEFINITION_REPRESENTATION(#33358,#33489);
#33308=SHAPE_DEFINITION_REPRESENTATION(#33359,#33490);
#33309=SHAPE_DEFINITION_REPRESENTATION(#33360,#33491);
#33310=SHAPE_DEFINITION_REPRESENTATION(#33361,#33492);
#33311=SHAPE_DEFINITION_REPRESENTATION(#33362,#33493);
#33312=SHAPE_DEFINITION_REPRESENTATION(#33363,#33494);
#33313=SHAPE_DEFINITION_REPRESENTATION(#33364,#33495);
#33314=SHAPE_DEFINITION_REPRESENTATION(#33365,#33496);
#33315=SHAPE_DEFINITION_REPRESENTATION(#33366,#33497);
#33316=SHAPE_DEFINITION_REPRESENTATION(#33367,#33498);
#33317=SHAPE_DEFINITION_REPRESENTATION(#33368,#33499);
#33318=SHAPE_DEFINITION_REPRESENTATION(#33369,#33500);
#33319=SHAPE_DEFINITION_REPRESENTATION(#33370,#33501);
#33320=SHAPE_DEFINITION_REPRESENTATION(#33371,#33502);
#33321=SHAPE_DEFINITION_REPRESENTATION(#33372,#33503);
#33322=SHAPE_DEFINITION_REPRESENTATION(#33373,#33504);
#33323=SHAPE_DEFINITION_REPRESENTATION(#33374,#33505);
#33324=SHAPE_DEFINITION_REPRESENTATION(#33375,#33506);
#33325=SHAPE_DEFINITION_REPRESENTATION(#33376,#33507);
#33326=SHAPE_DEFINITION_REPRESENTATION(#33377,#33508);
#33327=SHAPE_DEFINITION_REPRESENTATION(#33378,#33509);
#33328=SHAPE_DEFINITION_REPRESENTATION(#33379,#33510);
#33329=SHAPE_DEFINITION_REPRESENTATION(#33385,#33511);
#33330=SHAPE_DEFINITION_REPRESENTATION(#33386,#33512);
#33331=SHAPE_DEFINITION_REPRESENTATION(#33387,#33513);
#33332=SHAPE_DEFINITION_REPRESENTATION(#33388,#33514);
#33333=SHAPE_DEFINITION_REPRESENTATION(#33389,#33515);
#33334=SHAPE_DEFINITION_REPRESENTATION(#33390,#33516);
#33335=SHAPE_DEFINITION_REPRESENTATION(#33391,#33517);
#33336=SHAPE_DEFINITION_REPRESENTATION(#33392,#33518);
#33337=SHAPE_DEFINITION_REPRESENTATION(#33399,#33519);
#33338=SHAPE_DEFINITION_REPRESENTATION(#33400,#33520);
#33339=SHAPE_DEFINITION_REPRESENTATION(#33401,#33521);
#33340=SHAPE_DEFINITION_REPRESENTATION(#33402,#33522);
#33341=SHAPE_DEFINITION_REPRESENTATION(#33403,#33523);
#33342=SHAPE_DEFINITION_REPRESENTATION(#33404,#33524);
#33343=SHAPE_DEFINITION_REPRESENTATION(#33405,#33525);
#33344=SHAPE_DEFINITION_REPRESENTATION(#33406,#33526);
#33345=SHAPE_DEFINITION_REPRESENTATION(#33407,#33527);
#33346=SHAPE_DEFINITION_REPRESENTATION(#33408,#33528);
#33347=SHAPE_DEFINITION_REPRESENTATION(#33409,#33529);
#33348=SHAPE_DEFINITION_REPRESENTATION(#33410,#33530);
#33349=SHAPE_DEFINITION_REPRESENTATION(#33411,#33531);
#33350=SHAPE_DEFINITION_REPRESENTATION(#33412,#33532);
#33351=SHAPE_DEFINITION_REPRESENTATION(#33413,#33533);
#33352=SHAPE_DEFINITION_REPRESENTATION(#33414,#33534);
#33353=SHAPE_DEFINITION_REPRESENTATION(#33479,#33535);
#33354=SHAPE_DEFINITION_REPRESENTATION(#33480,#33536);
#33355=PRODUCT_DEFINITION_SHAPE('',$,#33538);
#33356=PRODUCT_DEFINITION_SHAPE('',$,#33539);
#33357=PRODUCT_DEFINITION_SHAPE('',$,#33540);
#33358=PRODUCT_DEFINITION_SHAPE('',$,#33541);
#33359=PRODUCT_DEFINITION_SHAPE('',$,#33542);
#33360=PRODUCT_DEFINITION_SHAPE('',$,#33543);
#33361=PRODUCT_DEFINITION_SHAPE('',$,#33544);
#33362=PRODUCT_DEFINITION_SHAPE('',$,#33545);
#33363=PRODUCT_DEFINITION_SHAPE('',$,#33546);
#33364=PRODUCT_DEFINITION_SHAPE('',$,#33547);
#33365=PRODUCT_DEFINITION_SHAPE('',$,#33548);
#33366=PRODUCT_DEFINITION_SHAPE('',$,#33549);
#33367=PRODUCT_DEFINITION_SHAPE('',$,#33550);
#33368=PRODUCT_DEFINITION_SHAPE('',$,#33551);
#33369=PRODUCT_DEFINITION_SHAPE('',$,#33552);
#33370=PRODUCT_DEFINITION_SHAPE('',$,#33553);
#33371=PRODUCT_DEFINITION_SHAPE('',$,#33554);
#33372=PRODUCT_DEFINITION_SHAPE('',$,#33555);
#33373=PRODUCT_DEFINITION_SHAPE('',$,#33556);
#33374=PRODUCT_DEFINITION_SHAPE('',$,#33557);
#33375=PRODUCT_DEFINITION_SHAPE('',$,#33558);
#33376=PRODUCT_DEFINITION_SHAPE('',$,#33559);
#33377=PRODUCT_DEFINITION_SHAPE('',$,#33560);
#33378=PRODUCT_DEFINITION_SHAPE('',$,#33561);
#33379=PRODUCT_DEFINITION_SHAPE('',$,#33562);
#33380=PRODUCT_DEFINITION_SHAPE($,$,#377);
#33381=PRODUCT_DEFINITION_SHAPE($,$,#378);
#33382=PRODUCT_DEFINITION_SHAPE($,$,#379);
#33383=PRODUCT_DEFINITION_SHAPE($,$,#380);
#33384=PRODUCT_DEFINITION_SHAPE($,$,#381);
#33385=PRODUCT_DEFINITION_SHAPE('',$,#33563);
#33386=PRODUCT_DEFINITION_SHAPE('',$,#33564);
#33387=PRODUCT_DEFINITION_SHAPE('',$,#33565);
#33388=PRODUCT_DEFINITION_SHAPE('',$,#33566);
#33389=PRODUCT_DEFINITION_SHAPE('',$,#33567);
#33390=PRODUCT_DEFINITION_SHAPE('',$,#33568);
#33391=PRODUCT_DEFINITION_SHAPE('',$,#33569);
#33392=PRODUCT_DEFINITION_SHAPE('',$,#33570);
#33393=PRODUCT_DEFINITION_SHAPE($,$,#382);
#33394=PRODUCT_DEFINITION_SHAPE($,$,#383);
#33395=PRODUCT_DEFINITION_SHAPE($,$,#384);
#33396=PRODUCT_DEFINITION_SHAPE($,$,#385);
#33397=PRODUCT_DEFINITION_SHAPE($,$,#386);
#33398=PRODUCT_DEFINITION_SHAPE($,$,#387);
#33399=PRODUCT_DEFINITION_SHAPE('',$,#33571);
#33400=PRODUCT_DEFINITION_SHAPE('',$,#33572);
#33401=PRODUCT_DEFINITION_SHAPE('',$,#33573);
#33402=PRODUCT_DEFINITION_SHAPE('',$,#33574);
#33403=PRODUCT_DEFINITION_SHAPE('',$,#33575);
#33404=PRODUCT_DEFINITION_SHAPE('',$,#33576);
#33405=PRODUCT_DEFINITION_SHAPE('',$,#33577);
#33406=PRODUCT_DEFINITION_SHAPE('',$,#33578);
#33407=PRODUCT_DEFINITION_SHAPE('',$,#33579);
#33408=PRODUCT_DEFINITION_SHAPE('',$,#33580);
#33409=PRODUCT_DEFINITION_SHAPE('',$,#33581);
#33410=PRODUCT_DEFINITION_SHAPE('',$,#33582);
#33411=PRODUCT_DEFINITION_SHAPE('',$,#33583);
#33412=PRODUCT_DEFINITION_SHAPE('',$,#33584);
#33413=PRODUCT_DEFINITION_SHAPE('',$,#33585);
#33414=PRODUCT_DEFINITION_SHAPE('',$,#33586);
#33415=PRODUCT_DEFINITION_SHAPE($,$,#388);
#33416=PRODUCT_DEFINITION_SHAPE($,$,#389);
#33417=PRODUCT_DEFINITION_SHAPE($,$,#390);
#33418=PRODUCT_DEFINITION_SHAPE($,$,#391);
#33419=PRODUCT_DEFINITION_SHAPE($,$,#392);
#33420=PRODUCT_DEFINITION_SHAPE($,$,#393);
#33421=PRODUCT_DEFINITION_SHAPE($,$,#394);
#33422=PRODUCT_DEFINITION_SHAPE($,$,#395);
#33423=PRODUCT_DEFINITION_SHAPE($,$,#396);
#33424=PRODUCT_DEFINITION_SHAPE($,$,#397);
#33425=PRODUCT_DEFINITION_SHAPE($,$,#398);
#33426=PRODUCT_DEFINITION_SHAPE($,$,#399);
#33427=PRODUCT_DEFINITION_SHAPE($,$,#400);
#33428=PRODUCT_DEFINITION_SHAPE($,$,#401);
#33429=PRODUCT_DEFINITION_SHAPE($,$,#402);
#33430=PRODUCT_DEFINITION_SHAPE($,$,#403);
#33431=PRODUCT_DEFINITION_SHAPE($,$,#404);
#33432=PRODUCT_DEFINITION_SHAPE($,$,#405);
#33433=PRODUCT_DEFINITION_SHAPE($,$,#406);
#33434=PRODUCT_DEFINITION_SHAPE($,$,#407);
#33435=PRODUCT_DEFINITION_SHAPE($,$,#408);
#33436=PRODUCT_DEFINITION_SHAPE($,$,#409);
#33437=PRODUCT_DEFINITION_SHAPE($,$,#410);
#33438=PRODUCT_DEFINITION_SHAPE($,$,#411);
#33439=PRODUCT_DEFINITION_SHAPE($,$,#412);
#33440=PRODUCT_DEFINITION_SHAPE($,$,#413);
#33441=PRODUCT_DEFINITION_SHAPE($,$,#414);
#33442=PRODUCT_DEFINITION_SHAPE($,$,#415);
#33443=PRODUCT_DEFINITION_SHAPE($,$,#416);
#33444=PRODUCT_DEFINITION_SHAPE($,$,#417);
#33445=PRODUCT_DEFINITION_SHAPE($,$,#418);
#33446=PRODUCT_DEFINITION_SHAPE($,$,#419);
#33447=PRODUCT_DEFINITION_SHAPE($,$,#420);
#33448=PRODUCT_DEFINITION_SHAPE($,$,#421);
#33449=PRODUCT_DEFINITION_SHAPE($,$,#422);
#33450=PRODUCT_DEFINITION_SHAPE($,$,#423);
#33451=PRODUCT_DEFINITION_SHAPE($,$,#424);
#33452=PRODUCT_DEFINITION_SHAPE($,$,#425);
#33453=PRODUCT_DEFINITION_SHAPE($,$,#426);
#33454=PRODUCT_DEFINITION_SHAPE($,$,#427);
#33455=PRODUCT_DEFINITION_SHAPE($,$,#428);
#33456=PRODUCT_DEFINITION_SHAPE($,$,#429);
#33457=PRODUCT_DEFINITION_SHAPE($,$,#430);
#33458=PRODUCT_DEFINITION_SHAPE($,$,#431);
#33459=PRODUCT_DEFINITION_SHAPE($,$,#432);
#33460=PRODUCT_DEFINITION_SHAPE($,$,#433);
#33461=PRODUCT_DEFINITION_SHAPE($,$,#434);
#33462=PRODUCT_DEFINITION_SHAPE($,$,#435);
#33463=PRODUCT_DEFINITION_SHAPE($,$,#436);
#33464=PRODUCT_DEFINITION_SHAPE($,$,#437);
#33465=PRODUCT_DEFINITION_SHAPE($,$,#438);
#33466=PRODUCT_DEFINITION_SHAPE($,$,#439);
#33467=PRODUCT_DEFINITION_SHAPE($,$,#440);
#33468=PRODUCT_DEFINITION_SHAPE($,$,#441);
#33469=PRODUCT_DEFINITION_SHAPE($,$,#442);
#33470=PRODUCT_DEFINITION_SHAPE($,$,#443);
#33471=PRODUCT_DEFINITION_SHAPE($,$,#444);
#33472=PRODUCT_DEFINITION_SHAPE($,$,#445);
#33473=PRODUCT_DEFINITION_SHAPE($,$,#446);
#33474=PRODUCT_DEFINITION_SHAPE($,$,#447);
#33475=PRODUCT_DEFINITION_SHAPE($,$,#448);
#33476=PRODUCT_DEFINITION_SHAPE($,$,#449);
#33477=PRODUCT_DEFINITION_SHAPE($,$,#450);
#33478=PRODUCT_DEFINITION_SHAPE($,$,#451);
#33479=PRODUCT_DEFINITION_SHAPE('',$,#33587);
#33480=PRODUCT_DEFINITION_SHAPE('',$,#33588);
#33481=PRODUCT_DEFINITION_SHAPE($,$,#452);
#33482=PRODUCT_DEFINITION_SHAPE($,$,#453);
#33483=PRODUCT_DEFINITION_SHAPE($,$,#454);
#33484=PRODUCT_DEFINITION_SHAPE($,$,#455);
#33485=PRODUCT_DEFINITION_SHAPE($,$,#456);
#33486=SHAPE_REPRESENTATION('',(#13188,#14363,#14364,#14365,#14366),#33248);
#33487=SHAPE_REPRESENTATION('',(#13189,#14288,#14289,#14290,#14291,#14292,
#14293,#14294,#14295,#14296,#14297,#14298,#14299,#14300,#14301,#14302,#14303,
#14304,#14305,#14306,#14307,#14308,#14309,#14310,#14311,#14312,#14313,#14314,
#14315,#14316,#14317,#14318,#14319,#14320,#14321,#14322,#14323,#14324,#14325,
#14326,#14327,#14328,#14329,#14330,#14331,#14332,#14333,#14334,#14335),
#33249);
#33488=SHAPE_REPRESENTATION('',(#13190),#33250);
#33489=SHAPE_REPRESENTATION('',(#13215),#33251);
#33490=SHAPE_REPRESENTATION('',(#13222),#33252);
#33491=SHAPE_REPRESENTATION('',(#13229),#33253);
#33492=SHAPE_REPRESENTATION('',(#13297),#33254);
#33493=SHAPE_REPRESENTATION('',(#13333),#33255);
#33494=SHAPE_REPRESENTATION('',(#13350),#33256);
#33495=SHAPE_REPRESENTATION('',(#13371),#33257);
#33496=SHAPE_REPRESENTATION('',(#13388),#33258);
#33497=SHAPE_REPRESENTATION('',(#13409),#33259);
#33498=SHAPE_REPRESENTATION('',(#13431),#33260);
#33499=SHAPE_REPRESENTATION('',(#13463),#33261);
#33500=SHAPE_REPRESENTATION('',(#13488),#33262);
#33501=SHAPE_REPRESENTATION('',(#13513),#33263);
#33502=SHAPE_REPRESENTATION('',(#13545),#33264);
#33503=SHAPE_REPRESENTATION('',(#13570),#33265);
#33504=SHAPE_REPRESENTATION('',(#13595),#33266);
#33505=SHAPE_REPRESENTATION('',(#13603,#13726,#13727,#13728,#13729,#13730),
#33267);
#33506=SHAPE_REPRESENTATION('',(#13604),#33268);
#33507=SHAPE_REPRESENTATION('',(#13624),#33269);
#33508=SHAPE_REPRESENTATION('',(#13644),#33270);
#33509=SHAPE_REPRESENTATION('',(#13659),#33271);
#33510=SHAPE_REPRESENTATION('',(#13709),#33272);
#33511=SHAPE_REPRESENTATION('',(#13731),#33273);
#33512=SHAPE_REPRESENTATION('',(#13755,#13998,#13999,#14000,#14001,#14002,
#14003),#33274);
#33513=SHAPE_REPRESENTATION('',(#13756),#33275);
#33514=SHAPE_REPRESENTATION('',(#13937),#33276);
#33515=SHAPE_REPRESENTATION('',(#13955),#33277);
#33516=SHAPE_REPRESENTATION('',(#13961),#33278);
#33517=SHAPE_REPRESENTATION('',(#13967),#33279);
#33518=SHAPE_REPRESENTATION('',(#13981),#33280);
#33519=SHAPE_REPRESENTATION('',(#14004,#14336,#14337,#14338,#14339,#14340,
#14341,#14342,#14343,#14344,#14345,#14346,#14347,#14348,#14349,#14350,#14351),
#33281);
#33520=SHAPE_REPRESENTATION('',(#14005),#33282);
#33521=SHAPE_REPRESENTATION('',(#14033),#33283);
#33522=SHAPE_REPRESENTATION('',(#14042),#33284);
#33523=SHAPE_REPRESENTATION('',(#14051),#33285);
#33524=SHAPE_REPRESENTATION('',(#14060),#33286);
#33525=SHAPE_REPRESENTATION('',(#14069),#33287);
#33526=SHAPE_REPRESENTATION('',(#14076),#33288);
#33527=SHAPE_REPRESENTATION('',(#14083),#33289);
#33528=SHAPE_REPRESENTATION('',(#14107),#33290);
#33529=SHAPE_REPRESENTATION('',(#14116),#33291);
#33530=SHAPE_REPRESENTATION('',(#14125),#33292);
#33531=SHAPE_REPRESENTATION('',(#14134),#33293);
#33532=SHAPE_REPRESENTATION('',(#14227),#33294);
#33533=SHAPE_REPRESENTATION('',(#14236),#33295);
#33534=SHAPE_REPRESENTATION('',(#14262),#33296);
#33535=SHAPE_REPRESENTATION('',(#14352,#14362),#33297);
#33536=SHAPE_REPRESENTATION('',(#14353),#33298);
#33537=PRODUCT_DEFINITION_CONTEXT('part definition',#33692,'design');
#33538=PRODUCT_DEFINITION('PAT-049','PAT-049',
#33589,#33537);
#33539=PRODUCT_DEFINITION('Column, head and worktable',
'Column, head and worktable',#33590,#33537);
#33540=PRODUCT_DEFINITION('Base','Base',#33591,#33537);
#33541=PRODUCT_DEFINITION('Foot strip','Foot strip',#33592,#33537);
#33542=PRODUCT_DEFINITION('Foot strip (1)','Foot strip (1)',#33593,#33537);
#33543=PRODUCT_DEFINITION('Head frame','Head frame',#33594,#33537);
#33544=PRODUCT_DEFINITION('Column socket','Column socket',#33595,#33537);
#33545=PRODUCT_DEFINITION('Split ram guide','Split ram guide',#33596,#33537);
#33546=PRODUCT_DEFINITION('Guide keeper','Guide keeper',#33597,#33537);
#33547=PRODUCT_DEFINITION('Split ram guide (1)','Split ram guide (1)',#33598,
#33537);
#33548=PRODUCT_DEFINITION('Guide keeper (1)','Guide keeper (1)',#33599,#33537);
#33549=PRODUCT_DEFINITION('Adjustable worktable','Adjustable worktable',
#33600,#33537);
#33550=PRODUCT_DEFINITION('Pinion bearing pedestal',
'Pinion bearing pedestal',#33601,#33537);
#33551=PRODUCT_DEFINITION('Pinion bearing cap','Pinion bearing cap',#33602,
#33537);
#33552=PRODUCT_DEFINITION('Pinion bearing cap (1)',
'Pinion bearing cap (1)',#33603,#33537);
#33553=PRODUCT_DEFINITION('Pinion bearing pedestal (1)',
'Pinion bearing pedestal (1)',#33604,#33537);
#33554=PRODUCT_DEFINITION('Pinion bearing cap (2)',
'Pinion bearing cap (2)',#33605,#33537);
#33555=PRODUCT_DEFINITION('Pinion bearing cap (3)',
'Pinion bearing cap (3)',#33606,#33537);
#33556=PRODUCT_DEFINITION('Column shaft 120 mm','Column shaft 120 mm',#33607,
#33537);
#33557=PRODUCT_DEFINITION('Sealed Ball Bearing - 12 x 32 x 10 mm',
'Sealed Ball Bearing - 12 x 32 x 10 mm',#33608,#33537);
#33558=PRODUCT_DEFINITION('Inner ring','Inner ring',#33609,#33537);
#33559=PRODUCT_DEFINITION('Outer ring','Outer ring',#33610,#33537);
#33560=PRODUCT_DEFINITION('Balls','Balls',#33611,#33537);
#33561=PRODUCT_DEFINITION('Cage','Cage',#33612,#33537);
#33562=PRODUCT_DEFINITION('Seals 2RS','Seals 2RS',#33613,#33537);
#33563=PRODUCT_DEFINITION('M4x10 Cap Screw','M4x10 Cap Screw',#33614,#33537);
#33564=PRODUCT_DEFINITION('Rack quill and tool holder',
'Rack quill and tool holder',#33615,#33537);
#33565=PRODUCT_DEFINITION('Rack quill','Rack quill',#33616,#33537);
#33566=PRODUCT_DEFINITION('Tool holder','Tool holder',#33617,#33537);
#33567=PRODUCT_DEFINITION('Tool shank envelope','Tool shank envelope',#33618,
#33537);
#33568=PRODUCT_DEFINITION('M4 tool retaining screw',
'M4 tool retaining screw',#33619,#33537);
#33569=PRODUCT_DEFINITION('Upper travel collar','Upper travel collar',#33620,
#33537);
#33570=PRODUCT_DEFINITION('Socket Set Screw - M4x6',
'Socket Set Screw - M4x6',#33621,#33537);
#33571=PRODUCT_DEFINITION('Pinion and operating lever',
'Pinion and operating lever',#33622,#33537);
#33572=PRODUCT_DEFINITION('Pinion shaft','Pinion shaft',#33623,#33537);
#33573=PRODUCT_DEFINITION('Inner race spacer 20 mm',
'Inner race spacer 20 mm',#33624,#33537);
#33574=PRODUCT_DEFINITION('Inner race spacer 15 mm',
'Inner race spacer 15 mm',#33625,#33537);
#33575=PRODUCT_DEFINITION('Inner race spacer 3 mm',
'Inner race spacer 3 mm',#33626,#33537);
#33576=PRODUCT_DEFINITION('Inner race spacer 15 mm (1)',
'Inner race spacer 15 mm (1)',#33627,#33537);
#33577=PRODUCT_DEFINITION('Parallel key 4 x 4 x 14 mm',
'Parallel key 4 x 4 x 14 mm',#33628,#33537);
#33578=PRODUCT_DEFINITION('Parallel key 4 x 4 x 14 mm (1)',
'Parallel key 4 x 4 x 14 mm (1)',#33629,#33537);
#33579=PRODUCT_DEFINITION('Operating lever','Operating lever',#33630,#33537);
#33580=PRODUCT_DEFINITION('Handle sleeve','Handle sleeve',#33631,#33537);
#33581=PRODUCT_DEFINITION('Shaft keeper','Shaft keeper',#33632,#33537);
#33582=PRODUCT_DEFINITION('Shaft keeper (1)','Shaft keeper (1)',#33633,#33537);
#33583=PRODUCT_DEFINITION('Spur Gear - Module 2, 20 Teeth, 12 mm Bore',
'Spur Gear - Module 2, 20 Teeth, 12 mm Bore',#33634,#33537);
#33584=PRODUCT_DEFINITION('Flat Washer - M6','Flat Washer - M6',#33635,
#33537);
#33585=PRODUCT_DEFINITION('Cap Screw - M6x25','Cap Screw - M6x25',#33636,
#33537);
#33586=PRODUCT_DEFINITION('Cap Screw - M4x16','Cap Screw - M4x16',#33637,
#33537);
#33587=PRODUCT_DEFINITION('Revolving hand grip','Revolving hand grip',#33638,
#33537);
#33588=PRODUCT_DEFINITION('Revolving grip','Revolving grip',#33639,#33537);
#33589=PRODUCT_DEFINITION_FORMATION('',$,#33694);
#33590=PRODUCT_DEFINITION_FORMATION('',$,#33695);
#33591=PRODUCT_DEFINITION_FORMATION('',$,#33696);
#33592=PRODUCT_DEFINITION_FORMATION('',$,#33697);
#33593=PRODUCT_DEFINITION_FORMATION('',$,#33698);
#33594=PRODUCT_DEFINITION_FORMATION('',$,#33699);
#33595=PRODUCT_DEFINITION_FORMATION('',$,#33700);
#33596=PRODUCT_DEFINITION_FORMATION('',$,#33701);
#33597=PRODUCT_DEFINITION_FORMATION('',$,#33702);
#33598=PRODUCT_DEFINITION_FORMATION('',$,#33703);
#33599=PRODUCT_DEFINITION_FORMATION('',$,#33704);
#33600=PRODUCT_DEFINITION_FORMATION('',$,#33705);
#33601=PRODUCT_DEFINITION_FORMATION('',$,#33706);
#33602=PRODUCT_DEFINITION_FORMATION('',$,#33707);
#33603=PRODUCT_DEFINITION_FORMATION('',$,#33708);
#33604=PRODUCT_DEFINITION_FORMATION('',$,#33709);
#33605=PRODUCT_DEFINITION_FORMATION('',$,#33710);
#33606=PRODUCT_DEFINITION_FORMATION('',$,#33711);
#33607=PRODUCT_DEFINITION_FORMATION('',$,#33712);
#33608=PRODUCT_DEFINITION_FORMATION('',$,#33713);
#33609=PRODUCT_DEFINITION_FORMATION('',$,#33714);
#33610=PRODUCT_DEFINITION_FORMATION('',$,#33715);
#33611=PRODUCT_DEFINITION_FORMATION('',$,#33716);
#33612=PRODUCT_DEFINITION_FORMATION('',$,#33717);
#33613=PRODUCT_DEFINITION_FORMATION('',$,#33718);
#33614=PRODUCT_DEFINITION_FORMATION('',$,#33719);
#33615=PRODUCT_DEFINITION_FORMATION('',$,#33720);
#33616=PRODUCT_DEFINITION_FORMATION('',$,#33721);
#33617=PRODUCT_DEFINITION_FORMATION('',$,#33722);
#33618=PRODUCT_DEFINITION_FORMATION('',$,#33723);
#33619=PRODUCT_DEFINITION_FORMATION('',$,#33724);
#33620=PRODUCT_DEFINITION_FORMATION('',$,#33725);
#33621=PRODUCT_DEFINITION_FORMATION('',$,#33726);
#33622=PRODUCT_DEFINITION_FORMATION('',$,#33727);
#33623=PRODUCT_DEFINITION_FORMATION('',$,#33728);
#33624=PRODUCT_DEFINITION_FORMATION('',$,#33729);
#33625=PRODUCT_DEFINITION_FORMATION('',$,#33730);
#33626=PRODUCT_DEFINITION_FORMATION('',$,#33731);
#33627=PRODUCT_DEFINITION_FORMATION('',$,#33732);
#33628=PRODUCT_DEFINITION_FORMATION('',$,#33733);
#33629=PRODUCT_DEFINITION_FORMATION('',$,#33734);
#33630=PRODUCT_DEFINITION_FORMATION('',$,#33735);
#33631=PRODUCT_DEFINITION_FORMATION('',$,#33736);
#33632=PRODUCT_DEFINITION_FORMATION('',$,#33737);
#33633=PRODUCT_DEFINITION_FORMATION('',$,#33738);
#33634=PRODUCT_DEFINITION_FORMATION('',$,#33739);
#33635=PRODUCT_DEFINITION_FORMATION('',$,#33740);
#33636=PRODUCT_DEFINITION_FORMATION('',$,#33741);
#33637=PRODUCT_DEFINITION_FORMATION('',$,#33742);
#33638=PRODUCT_DEFINITION_FORMATION('',$,#33743);
#33639=PRODUCT_DEFINITION_FORMATION('',$,#33744);
#33640=PRODUCT_RELATED_PRODUCT_CATEGORY('PAT-049','PAT-049',(#33694));
#33641=PRODUCT_RELATED_PRODUCT_CATEGORY('Column, head and worktable',
'Column, head and worktable',(#33695));
#33642=PRODUCT_RELATED_PRODUCT_CATEGORY('Base','Base',(#33696));
#33643=PRODUCT_RELATED_PRODUCT_CATEGORY('Foot strip','Foot strip',(#33697));
#33644=PRODUCT_RELATED_PRODUCT_CATEGORY('Foot strip (1)',
'Foot strip (1)',(#33698));
#33645=PRODUCT_RELATED_PRODUCT_CATEGORY('Head frame','Head frame',(#33699));
#33646=PRODUCT_RELATED_PRODUCT_CATEGORY('Column socket','Column socket',
(#33700));
#33647=PRODUCT_RELATED_PRODUCT_CATEGORY('Split ram guide',
'Split ram guide',(#33701));
#33648=PRODUCT_RELATED_PRODUCT_CATEGORY('Guide keeper','Guide keeper',(#33702));
#33649=PRODUCT_RELATED_PRODUCT_CATEGORY('Split ram guide (1)',
'Split ram guide (1)',(#33703));
#33650=PRODUCT_RELATED_PRODUCT_CATEGORY('Guide keeper (1)',
'Guide keeper (1)',(#33704));
#33651=PRODUCT_RELATED_PRODUCT_CATEGORY('Adjustable worktable',
'Adjustable worktable',(#33705));
#33652=PRODUCT_RELATED_PRODUCT_CATEGORY('Pinion bearing pedestal',
'Pinion bearing pedestal',(#33706));
#33653=PRODUCT_RELATED_PRODUCT_CATEGORY('Pinion bearing cap',
'Pinion bearing cap',(#33707));
#33654=PRODUCT_RELATED_PRODUCT_CATEGORY('Pinion bearing cap (1)',
'Pinion bearing cap (1)',(#33708));
#33655=PRODUCT_RELATED_PRODUCT_CATEGORY('Pinion bearing pedestal (1)',
'Pinion bearing pedestal (1)',(#33709));
#33656=PRODUCT_RELATED_PRODUCT_CATEGORY('Pinion bearing cap (2)',
'Pinion bearing cap (2)',(#33710));
#33657=PRODUCT_RELATED_PRODUCT_CATEGORY('Pinion bearing cap (3)',
'Pinion bearing cap (3)',(#33711));
#33658=PRODUCT_RELATED_PRODUCT_CATEGORY('Column shaft 120 mm',
'Column shaft 120 mm',(#33712));
#33659=PRODUCT_RELATED_PRODUCT_CATEGORY(
'Sealed Ball Bearing - 12 x 32 x 10 mm',
'Sealed Ball Bearing - 12 x 32 x 10 mm',(#33713));
#33660=PRODUCT_RELATED_PRODUCT_CATEGORY('Inner ring','Inner ring',(#33714));
#33661=PRODUCT_RELATED_PRODUCT_CATEGORY('Outer ring','Outer ring',(#33715));
#33662=PRODUCT_RELATED_PRODUCT_CATEGORY('Balls','Balls',(#33716));
#33663=PRODUCT_RELATED_PRODUCT_CATEGORY('Cage','Cage',(#33717));
#33664=PRODUCT_RELATED_PRODUCT_CATEGORY('Seals 2RS','Seals 2RS',(#33718));
#33665=PRODUCT_RELATED_PRODUCT_CATEGORY('M4x10 Cap Screw',
'M4x10 Cap Screw',(#33719));
#33666=PRODUCT_RELATED_PRODUCT_CATEGORY('Rack quill and tool holder',
'Rack quill and tool holder',(#33720));
#33667=PRODUCT_RELATED_PRODUCT_CATEGORY('Rack quill','Rack quill',(#33721));
#33668=PRODUCT_RELATED_PRODUCT_CATEGORY('Tool holder','Tool holder',(#33722));
#33669=PRODUCT_RELATED_PRODUCT_CATEGORY('Tool shank envelope',
'Tool shank envelope',(#33723));
#33670=PRODUCT_RELATED_PRODUCT_CATEGORY('M4 tool retaining screw',
'M4 tool retaining screw',(#33724));
#33671=PRODUCT_RELATED_PRODUCT_CATEGORY('Upper travel collar',
'Upper travel collar',(#33725));
#33672=PRODUCT_RELATED_PRODUCT_CATEGORY('Socket Set Screw - M4x6',
'Socket Set Screw - M4x6',(#33726));
#33673=PRODUCT_RELATED_PRODUCT_CATEGORY('Pinion and operating lever',
'Pinion and operating lever',(#33727));
#33674=PRODUCT_RELATED_PRODUCT_CATEGORY('Pinion shaft','Pinion shaft',(#33728));
#33675=PRODUCT_RELATED_PRODUCT_CATEGORY('Inner race spacer 20 mm',
'Inner race spacer 20 mm',(#33729));
#33676=PRODUCT_RELATED_PRODUCT_CATEGORY('Inner race spacer 15 mm',
'Inner race spacer 15 mm',(#33730));
#33677=PRODUCT_RELATED_PRODUCT_CATEGORY('Inner race spacer 3 mm',
'Inner race spacer 3 mm',(#33731));
#33678=PRODUCT_RELATED_PRODUCT_CATEGORY('Inner race spacer 15 mm (1)',
'Inner race spacer 15 mm (1)',(#33732));
#33679=PRODUCT_RELATED_PRODUCT_CATEGORY('Parallel key 4 x 4 x 14 mm',
'Parallel key 4 x 4 x 14 mm',(#33733));
#33680=PRODUCT_RELATED_PRODUCT_CATEGORY(
'Parallel key 4 x 4 x 14 mm (1)','Parallel key 4 x 4 x 14 mm (1)',(#33734));
#33681=PRODUCT_RELATED_PRODUCT_CATEGORY('Operating lever',
'Operating lever',(#33735));
#33682=PRODUCT_RELATED_PRODUCT_CATEGORY('Handle sleeve','Handle sleeve',
(#33736));
#33683=PRODUCT_RELATED_PRODUCT_CATEGORY('Shaft keeper','Shaft keeper',(#33737));
#33684=PRODUCT_RELATED_PRODUCT_CATEGORY('Shaft keeper (1)',
'Shaft keeper (1)',(#33738));
#33685=PRODUCT_RELATED_PRODUCT_CATEGORY(
'Spur Gear - Module 2, 20 Teeth, 12 mm Bore',
'Spur Gear - Module 2, 20 Teeth, 12 mm Bore',(#33739));
#33686=PRODUCT_RELATED_PRODUCT_CATEGORY('Flat Washer - M6',
'Flat Washer - M6',(#33740));
#33687=PRODUCT_RELATED_PRODUCT_CATEGORY('Cap Screw - M6x25',
'Cap Screw - M6x25',(#33741));
#33688=PRODUCT_RELATED_PRODUCT_CATEGORY('Cap Screw - M4x16',
'Cap Screw - M4x16',(#33742));
#33689=PRODUCT_RELATED_PRODUCT_CATEGORY('Revolving hand grip',
'Revolving hand grip',(#33743));
#33690=PRODUCT_RELATED_PRODUCT_CATEGORY('Revolving grip',
'Revolving grip',(#33744));
#33691=APPLICATION_PROTOCOL_DEFINITION('international standard',
'automotive_design',2009,#33692);
#33692=APPLICATION_CONTEXT(
'Core Data for Automotive Mechanical Design Process');
#33693=PRODUCT_CONTEXT('part definition',#33692,'mechanical');
#33694=PRODUCT('PAT-049','PAT-049',
'PAT-049',(#33693));
#33695=PRODUCT('Column, head and worktable',
'Column, head and worktable','Column, head and worktable',(#33693));
#33696=PRODUCT('Base','Base','Base',(#33693));
#33697=PRODUCT('Foot strip','Foot strip','Foot strip',(#33693));
#33698=PRODUCT('Foot strip (1)','Foot strip (1)','Foot strip (1)',(#33693));
#33699=PRODUCT('Head frame','Head frame','Head frame',(#33693));
#33700=PRODUCT('Column socket','Column socket','Column socket',(#33693));
#33701=PRODUCT('Split ram guide','Split ram guide','Split ram guide',(#33693));
#33702=PRODUCT('Guide keeper','Guide keeper','Guide keeper',(#33693));
#33703=PRODUCT('Split ram guide (1)','Split ram guide (1)',
'Split ram guide (1)',(#33693));
#33704=PRODUCT('Guide keeper (1)','Guide keeper (1)','Guide keeper (1)',(#33693));
#33705=PRODUCT('Adjustable worktable','Adjustable worktable',
'Adjustable worktable',(#33693));
#33706=PRODUCT('Pinion bearing pedestal','Pinion bearing pedestal',
'Pinion bearing pedestal',(#33693));
#33707=PRODUCT('Pinion bearing cap','Pinion bearing cap',
'Pinion bearing cap',(#33693));
#33708=PRODUCT('Pinion bearing cap (1)','Pinion bearing cap (1)',
'Pinion bearing cap (1)',(#33693));
#33709=PRODUCT('Pinion bearing pedestal (1)',
'Pinion bearing pedestal (1)','Pinion bearing pedestal (1)',(#33693));
#33710=PRODUCT('Pinion bearing cap (2)','Pinion bearing cap (2)',
'Pinion bearing cap (2)',(#33693));
#33711=PRODUCT('Pinion bearing cap (3)','Pinion bearing cap (3)',
'Pinion bearing cap (3)',(#33693));
#33712=PRODUCT('Column shaft 120 mm','Column shaft 120 mm',
'Column shaft 120 mm',(#33693));
#33713=PRODUCT('Sealed Ball Bearing - 12 x 32 x 10 mm',
'Sealed Ball Bearing - 12 x 32 x 10 mm',
'Sealed Ball Bearing - 12 x 32 x 10 mm',(#33693));
#33714=PRODUCT('Inner ring','Inner ring','Inner ring',(#33693));
#33715=PRODUCT('Outer ring','Outer ring','Outer ring',(#33693));
#33716=PRODUCT('Balls','Balls','Balls',(#33693));
#33717=PRODUCT('Cage','Cage','Cage',(#33693));
#33718=PRODUCT('Seals 2RS','Seals 2RS','Seals 2RS',(#33693));
#33719=PRODUCT('M4x10 Cap Screw','M4x10 Cap Screw','M4x10 Cap Screw',(#33693));
#33720=PRODUCT('Rack quill and tool holder',
'Rack quill and tool holder','Rack quill and tool holder',(#33693));
#33721=PRODUCT('Rack quill','Rack quill','Rack quill',(#33693));
#33722=PRODUCT('Tool holder','Tool holder','Tool holder',(#33693));
#33723=PRODUCT('Tool shank envelope','Tool shank envelope',
'Tool shank envelope',(#33693));
#33724=PRODUCT('M4 tool retaining screw','M4 tool retaining screw',
'M4 tool retaining screw',(#33693));
#33725=PRODUCT('Upper travel collar','Upper travel collar',
'Upper travel collar',(#33693));
#33726=PRODUCT('Socket Set Screw - M4x6','Socket Set Screw - M4x6',
'Socket Set Screw - M4x6',(#33693));
#33727=PRODUCT('Pinion and operating lever',
'Pinion and operating lever','Pinion and operating lever',(#33693));
#33728=PRODUCT('Pinion shaft','Pinion shaft','Pinion shaft',(#33693));
#33729=PRODUCT('Inner race spacer 20 mm','Inner race spacer 20 mm',
'Inner race spacer 20 mm',(#33693));
#33730=PRODUCT('Inner race spacer 15 mm','Inner race spacer 15 mm',
'Inner race spacer 15 mm',(#33693));
#33731=PRODUCT('Inner race spacer 3 mm','Inner race spacer 3 mm',
'Inner race spacer 3 mm',(#33693));
#33732=PRODUCT('Inner race spacer 15 mm (1)',
'Inner race spacer 15 mm (1)','Inner race spacer 15 mm (1)',(#33693));
#33733=PRODUCT('Parallel key 4 x 4 x 14 mm',
'Parallel key 4 x 4 x 14 mm','Parallel key 4 x 4 x 14 mm',(#33693));
#33734=PRODUCT('Parallel key 4 x 4 x 14 mm (1)',
'Parallel key 4 x 4 x 14 mm (1)','Parallel key 4 x 4 x 14 mm (1)',(#33693));
#33735=PRODUCT('Operating lever','Operating lever','Operating lever',(#33693));
#33736=PRODUCT('Handle sleeve','Handle sleeve','Handle sleeve',(#33693));
#33737=PRODUCT('Shaft keeper','Shaft keeper','Shaft keeper',(#33693));
#33738=PRODUCT('Shaft keeper (1)','Shaft keeper (1)','Shaft keeper (1)',(#33693));
#33739=PRODUCT('Spur Gear - Module 2, 20 Teeth, 12 mm Bore',
'Spur Gear - Module 2, 20 Teeth, 12 mm Bore',
'Spur Gear - Module 2, 20 Teeth, 12 mm Bore',(#33693));
#33740=PRODUCT('Flat Washer - M6','Flat Washer - M6','Flat Washer - M6',
(#33693));
#33741=PRODUCT('Cap Screw - M6x25','Cap Screw - M6x25',
'Cap Screw - M6x25',(#33693));
#33742=PRODUCT('Cap Screw - M4x16','Cap Screw - M4x16',
'Cap Screw - M4x16',(#33693));
#33743=PRODUCT('Revolving hand grip','Revolving hand grip',
'Revolving hand grip',(#33693));
#33744=PRODUCT('Revolving grip','Revolving grip','Revolving grip',(#33693));
#33745=PRESENTATION_STYLE_ASSIGNMENT((#33751));
#33746=PRESENTATION_STYLE_ASSIGNMENT((#33752));
#33747=PRESENTATION_STYLE_ASSIGNMENT((#33753));
#33748=PRESENTATION_STYLE_ASSIGNMENT((#33754));
#33749=PRESENTATION_STYLE_ASSIGNMENT((#33755));
#33750=PRESENTATION_STYLE_ASSIGNMENT((#33756));
#33751=SURFACE_STYLE_USAGE(.BOTH.,#33757);
#33752=SURFACE_STYLE_USAGE(.BOTH.,#33758);
#33753=SURFACE_STYLE_USAGE(.BOTH.,#33759);
#33754=SURFACE_STYLE_USAGE(.BOTH.,#33760);
#33755=SURFACE_STYLE_USAGE(.BOTH.,#33761);
#33756=SURFACE_STYLE_USAGE(.BOTH.,#33762);
#33757=SURFACE_SIDE_STYLE('',(#33763));
#33758=SURFACE_SIDE_STYLE('',(#33764));
#33759=SURFACE_SIDE_STYLE('',(#33765));
#33760=SURFACE_SIDE_STYLE('',(#33766));
#33761=SURFACE_SIDE_STYLE('',(#33767));
#33762=SURFACE_SIDE_STYLE('',(#33768));
#33763=SURFACE_STYLE_FILL_AREA(#33769);
#33764=SURFACE_STYLE_FILL_AREA(#33770);
#33765=SURFACE_STYLE_FILL_AREA(#33771);
#33766=SURFACE_STYLE_FILL_AREA(#33772);
#33767=SURFACE_STYLE_FILL_AREA(#33773);
#33768=SURFACE_STYLE_FILL_AREA(#33774);
#33769=FILL_AREA_STYLE('Steel - Satin',(#33775));
#33770=FILL_AREA_STYLE('CAD Library Painted - Deep blue',(#33776));
#33771=FILL_AREA_STYLE('CAD Library Painted - Engineering blue',(#33777));
#33772=FILL_AREA_STYLE('CAD Library Painted - Light blue',(#33778));
#33773=FILL_AREA_STYLE('CAD Library Painted - Steel gray',(#33779));
#33774=FILL_AREA_STYLE('CAD Library Painted - Graphite',(#33780));
#33775=FILL_AREA_STYLE_COLOUR('Steel - Satin',#33781);
#33776=FILL_AREA_STYLE_COLOUR('CAD Library Painted - Deep blue',#33782);
#33777=FILL_AREA_STYLE_COLOUR('CAD Library Painted - Engineering blue',
#33783);
#33778=FILL_AREA_STYLE_COLOUR('CAD Library Painted - Light blue',#33784);
#33779=FILL_AREA_STYLE_COLOUR('CAD Library Painted - Steel gray',#33785);
#33780=FILL_AREA_STYLE_COLOUR('CAD Library Painted - Graphite',#33786);
#33781=COLOUR_RGB('Steel - Satin',0.627450980392157,0.627450980392157,0.627450980392157);
#33782=COLOUR_RGB('CAD Library Painted - Deep blue',0.0784313725490196,
0.203921568627451,0.349019607843137);
#33783=COLOUR_RGB('CAD Library Painted - Engineering blue',0.12156862745098,
0.356862745098039,0.6);
#33784=COLOUR_RGB('CAD Library Painted - Light blue',0.286274509803922,
0.552941176470588,0.780392156862745);
#33785=COLOUR_RGB('CAD Library Painted - Steel gray',0.592156862745098,
0.631372549019608,0.67843137254902);
#33786=COLOUR_RGB('CAD Library Painted - Graphite',0.168627450980392,0.192156862745098,
0.231372549019608);
#33787=COLOUR_RGB('Dark Blue',0.08,0.2,0.34);
#33788=FILL_AREA_STYLE_COLOUR('',#33787);
#33789=FILL_AREA_STYLE('',(#33788));
#33790=SURFACE_STYLE_FILL_AREA(#33789);
#33791=SURFACE_SIDE_STYLE('',(#33790));
#33792=SURFACE_STYLE_USAGE(.BOTH.,#33791);
#33793=PRESENTATION_STYLE_ASSIGNMENT((#33792));
#33794=COLOUR_RGB('Light Blue',0.38,0.62,0.78);
#33795=FILL_AREA_STYLE_COLOUR('',#33794);
#33796=FILL_AREA_STYLE('',(#33795));
#33797=SURFACE_STYLE_FILL_AREA(#33796);
#33798=SURFACE_SIDE_STYLE('',(#33797));
#33799=SURFACE_STYLE_USAGE(.BOTH.,#33798);
#33800=PRESENTATION_STYLE_ASSIGNMENT((#33799));
#33801=COLOUR_RGB('Sky Blue',0.24,0.69,0.87);
#33802=FILL_AREA_STYLE_COLOUR('',#33801);
#33803=FILL_AREA_STYLE('',(#33802));
#33804=SURFACE_STYLE_FILL_AREA(#33803);
#33805=SURFACE_SIDE_STYLE('',(#33804));
#33806=SURFACE_STYLE_USAGE(.BOTH.,#33805);
#33807=PRESENTATION_STYLE_ASSIGNMENT((#33806));
#33808=COLOUR_RGB('Grey',0.48,0.52,0.57);
#33809=FILL_AREA_STYLE_COLOUR('',#33808);
#33810=FILL_AREA_STYLE('',(#33809));
#33811=SURFACE_STYLE_FILL_AREA(#33810);
#33812=SURFACE_SIDE_STYLE('',(#33811));
#33813=SURFACE_STYLE_USAGE(.BOTH.,#33812);
#33814=PRESENTATION_STYLE_ASSIGNMENT((#33813));
#33815=COLOUR_RGB('Black',0.12,0.14,0.17);
#33816=FILL_AREA_STYLE_COLOUR('',#33815);
#33817=FILL_AREA_STYLE('',(#33816));
#33818=SURFACE_STYLE_FILL_AREA(#33817);
#33819=SURFACE_SIDE_STYLE('',(#33818));
#33820=SURFACE_STYLE_USAGE(.BOTH.,#33819);
#33821=PRESENTATION_STYLE_ASSIGNMENT((#33820));
#33822=COLOUR_RGB('Off White',0.89,0.88,0.83);
#33823=FILL_AREA_STYLE_COLOUR('',#33822);
#33824=FILL_AREA_STYLE('',(#33823));
#33825=SURFACE_STYLE_FILL_AREA(#33824);
#33826=SURFACE_SIDE_STYLE('',(#33825));
#33827=SURFACE_STYLE_USAGE(.BOTH.,#33826);
#33828=PRESENTATION_STYLE_ASSIGNMENT((#33827));
ENDSEC;
END-ISO-10303-21;
